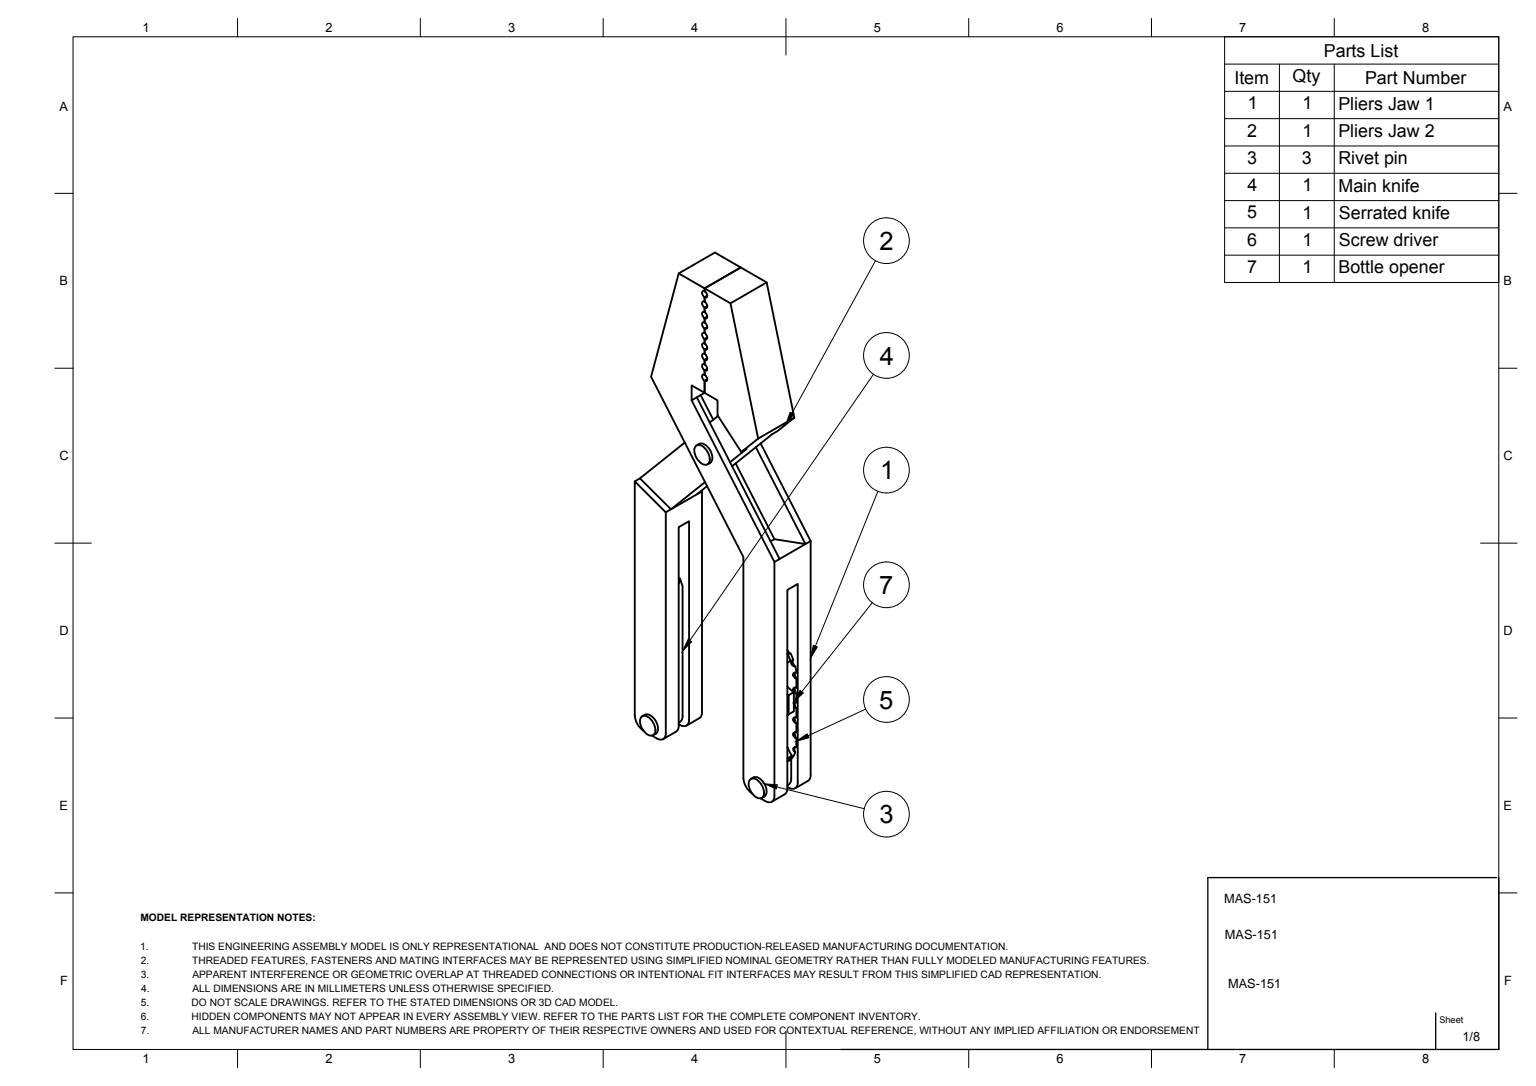
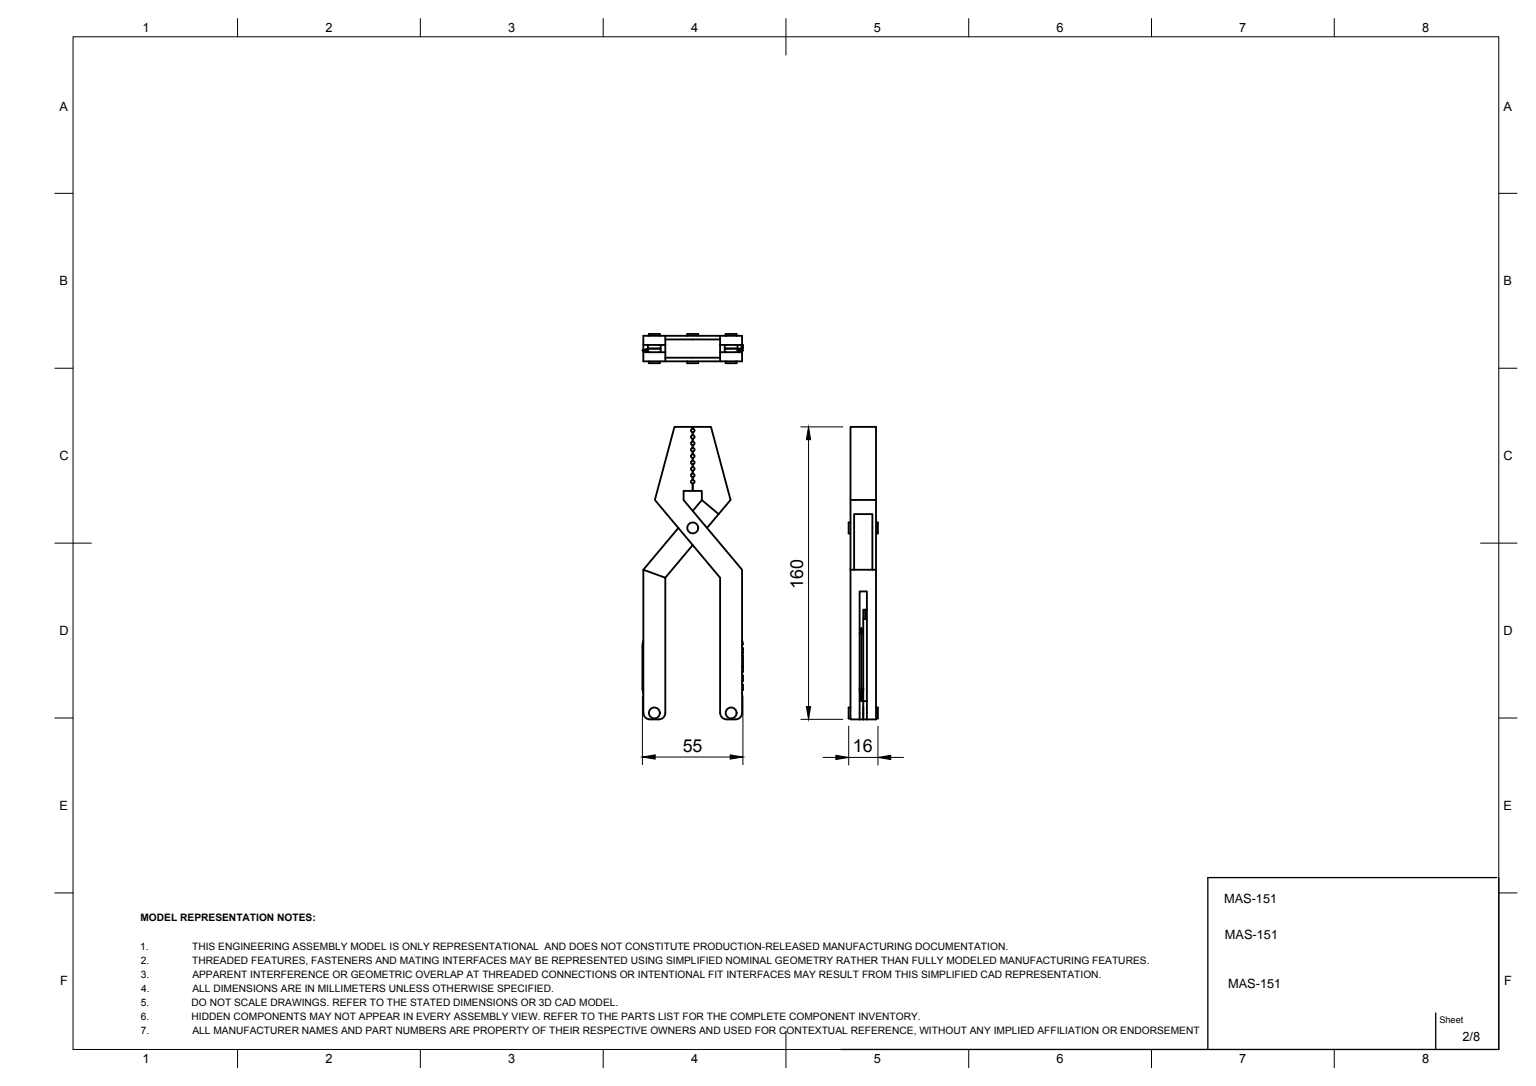
ISO-10303-21;
HEADER;
/* Generated by software containing ST-Developer
 * from STEP Tools, Inc. (www.steptools.com) 
 */

FILE_DESCRIPTION(
/* description */ ('STEP AP214'),
/* implementation_level */ '2;1');

FILE_NAME(
/* name */ 'MAS-151',
/* time_stamp */ '2026-11-04T19:14:12-08:00',
/* author */ (''),
/* organization */ (''),
/* preprocessor_version */ 'ST-DEVELOPER v20.2',
/* originating_system */ 'Autodesk Translation Framework v15.17.0.0',
/* authorisation */ '');

FILE_SCHEMA (('AUTOMOTIVE_DESIGN { 1 0 10303 214 3 1 1 }'));
ENDSEC;

DATA;
#10=MECHANICAL_DESIGN_GEOMETRIC_PRESENTATION_REPRESENTATION('',(#99,#100,
#101,#102,#103,#104,#105),#5990);
#11=ITEM_DEFINED_TRANSFORMATION($,$,#3355,#3676);
#12=ITEM_DEFINED_TRANSFORMATION($,$,#3437,#3677);
#13=ITEM_DEFINED_TRANSFORMATION($,$,#3662,#3678);
#14=ITEM_DEFINED_TRANSFORMATION($,$,#3519,#3679);
#15=ITEM_DEFINED_TRANSFORMATION($,$,#3540,#3680);
#16=ITEM_DEFINED_TRANSFORMATION($,$,#3585,#3681);
#17=ITEM_DEFINED_TRANSFORMATION($,$,#3638,#3682);
#18=ITEM_DEFINED_TRANSFORMATION($,$,#3662,#3683);
#19=ITEM_DEFINED_TRANSFORMATION($,$,#3662,#3684);
#20=(
REPRESENTATION_RELATIONSHIP($,$,#6021,#6020)
REPRESENTATION_RELATIONSHIP_WITH_TRANSFORMATION(#11)
SHAPE_REPRESENTATION_RELATIONSHIP()
);
#21=(
REPRESENTATION_RELATIONSHIP($,$,#6022,#6020)
REPRESENTATION_RELATIONSHIP_WITH_TRANSFORMATION(#12)
SHAPE_REPRESENTATION_RELATIONSHIP()
);
#22=(
REPRESENTATION_RELATIONSHIP($,$,#6027,#6020)
REPRESENTATION_RELATIONSHIP_WITH_TRANSFORMATION(#13)
SHAPE_REPRESENTATION_RELATIONSHIP()
);
#23=(
REPRESENTATION_RELATIONSHIP($,$,#6023,#6020)
REPRESENTATION_RELATIONSHIP_WITH_TRANSFORMATION(#14)
SHAPE_REPRESENTATION_RELATIONSHIP()
);
#24=(
REPRESENTATION_RELATIONSHIP($,$,#6024,#6020)
REPRESENTATION_RELATIONSHIP_WITH_TRANSFORMATION(#15)
SHAPE_REPRESENTATION_RELATIONSHIP()
);
#25=(
REPRESENTATION_RELATIONSHIP($,$,#6025,#6020)
REPRESENTATION_RELATIONSHIP_WITH_TRANSFORMATION(#16)
SHAPE_REPRESENTATION_RELATIONSHIP()
);
#26=(
REPRESENTATION_RELATIONSHIP($,$,#6026,#6020)
REPRESENTATION_RELATIONSHIP_WITH_TRANSFORMATION(#17)
SHAPE_REPRESENTATION_RELATIONSHIP()
);
#27=(
REPRESENTATION_RELATIONSHIP($,$,#6027,#6020)
REPRESENTATION_RELATIONSHIP_WITH_TRANSFORMATION(#18)
SHAPE_REPRESENTATION_RELATIONSHIP()
);
#28=(
REPRESENTATION_RELATIONSHIP($,$,#6027,#6020)
REPRESENTATION_RELATIONSHIP_WITH_TRANSFORMATION(#19)
SHAPE_REPRESENTATION_RELATIONSHIP()
);
#29=CONTEXT_DEPENDENT_SHAPE_REPRESENTATION(#20,#6011);
#30=CONTEXT_DEPENDENT_SHAPE_REPRESENTATION(#21,#6012);
#31=CONTEXT_DEPENDENT_SHAPE_REPRESENTATION(#22,#6013);
#32=CONTEXT_DEPENDENT_SHAPE_REPRESENTATION(#23,#6014);
#33=CONTEXT_DEPENDENT_SHAPE_REPRESENTATION(#24,#6015);
#34=CONTEXT_DEPENDENT_SHAPE_REPRESENTATION(#25,#6016);
#35=CONTEXT_DEPENDENT_SHAPE_REPRESENTATION(#26,#6017);
#36=CONTEXT_DEPENDENT_SHAPE_REPRESENTATION(#27,#6018);
#37=CONTEXT_DEPENDENT_SHAPE_REPRESENTATION(#28,#6019);
#38=NEXT_ASSEMBLY_USAGE_OCCURRENCE('Pliers Jaw 1:1','Pliers Jaw 1:1',
'Pliers Jaw 1:1',#6029,#6030,'Pliers Jaw 1:1');
#39=NEXT_ASSEMBLY_USAGE_OCCURRENCE('Pliers Jaw 2:1','Pliers Jaw 2:1',
'Pliers Jaw 2:1',#6029,#6031,'Pliers Jaw 2:1');
#40=NEXT_ASSEMBLY_USAGE_OCCURRENCE('rivet pin:1','rivet pin:1',
'rivet pin:1',#6029,#6036,'rivet pin:1');
#41=NEXT_ASSEMBLY_USAGE_OCCURRENCE('main knife:1','main knife:1',
'main knife:1',#6029,#6032,'main knife:1');
#42=NEXT_ASSEMBLY_USAGE_OCCURRENCE('serrated knife:1',
'serrated knife:1','serrated knife:1',#6029,#6033,'serrated knife:1');
#43=NEXT_ASSEMBLY_USAGE_OCCURRENCE('screw driver:1','screw driver:1',
'screw driver:1',#6029,#6034,'screw driver:1');
#44=NEXT_ASSEMBLY_USAGE_OCCURRENCE('bottle opener:1','bottle opener:1',
'bottle opener:1',#6029,#6035,'bottle opener:1');
#45=NEXT_ASSEMBLY_USAGE_OCCURRENCE('rivet pin:2','rivet pin:2',
'rivet pin:2',#6029,#6036,'rivet pin:2');
#46=NEXT_ASSEMBLY_USAGE_OCCURRENCE('rivet pin:3','rivet pin:3',
'rivet pin:3',#6029,#6036,'rivet pin:3');
#47=(
BOUNDED_SURFACE()
B_SPLINE_SURFACE(3,2,((#5769,#5770,#5771),(#5772,#5773,#5774),(#5775,#5776,
#5777),(#5778,#5779,#5780),(#5781,#5782,#5783),(#5784,#5785,#5786),(#5787,
#5788,#5789),(#5790,#5791,#5792),(#5793,#5794,#5795),(#5796,#5797,#5798),
(#5799,#5800,#5801),(#5802,#5803,#5804),(#5805,#5806,#5807),(#5808,#5809,
#5810),(#5811,#5812,#5813),(#5814,#5815,#5816),(#5817,#5818,#5819),(#5820,
#5821,#5822)),.UNSPECIFIED.,.F.,.F.,.F.)
B_SPLINE_SURFACE_WITH_KNOTS((4,2,2,2,2,2,2,2,4),(3,3),(0.00467154358091484,
0.00499795425216117,0.00521234917938639,0.00542674410661162,0.00564113903383685,
0.00585553396106207,0.0060699288882873,0.00628432381551252,0.00661073448675885),
(0.,1.00011201574402),.UNSPECIFIED.)
GEOMETRIC_REPRESENTATION_ITEM()
RATIONAL_B_SPLINE_SURFACE(((1.,0.701778016251575,1.00006681111479),(1.,
0.706507936356085,1.00006575146375),(1.,0.712393708374132,1.00006443286548),
(1.,0.724799452378116,1.00006165358819),(1.,0.730457055067376,1.00006038610704),
(1.,0.742658843750505,1.00005765252217),(1.,0.749286323952398,1.00005616775792),
(1.,0.759971140951244,1.00005377402247),(1.,0.763704964258696,1.00005293752847),
(1.,0.763766920917064,1.00005292364823),(1.,0.760086272902725,1.00005374822928),
(1.,0.74942657380375,1.00005613633753),(1.,0.742780641856394,1.00005762523556),
(1.,0.730540791311145,1.00006036734749),(1.,0.724865847327457,1.00006163871363),
(1.,0.712422254236158,1.00006442647031),(1.,0.706506681063795,1.00006575174497),
(1.,0.701749277073212,1.00006681755327)))
REPRESENTATION_ITEM('')
SURFACE()
);
#48=(
BOUNDED_SURFACE()
B_SPLINE_SURFACE(3,2,((#5827,#5828,#5829),(#5830,#5831,#5832),(#5833,#5834,
#5835),(#5836,#5837,#5838),(#5839,#5840,#5841),(#5842,#5843,#5844),(#5845,
#5846,#5847),(#5848,#5849,#5850),(#5851,#5852,#5853),(#5854,#5855,#5856),
(#5857,#5858,#5859),(#5860,#5861,#5862),(#5863,#5864,#5865),(#5866,#5867,
#5868),(#5869,#5870,#5871),(#5872,#5873,#5874),(#5875,#5876,#5877),(#5878,
#5879,#5880)),.UNSPECIFIED.,.F.,.F.,.F.)
B_SPLINE_SURFACE_WITH_KNOTS((4,2,2,2,2,2,2,2,4),(3,3),(0.00467154358091712,
0.00499795425216117,0.0052123491793864,0.00542674410661162,0.00564113903383685,
0.00585553396106207,0.0060699288882873,0.00628432381551253,0.00661073448675658),
(0.,1.00011201574402),.UNSPECIFIED.)
GEOMETRIC_REPRESENTATION_ITEM()
RATIONAL_B_SPLINE_SURFACE(((1.,0.701778016251691,1.00006681111478),(1.,
0.706507936356154,1.00006575146375),(1.,0.712393708374192,1.00006443286548),
(1.,0.724799452378113,1.00006165358819),(1.,0.730457055067361,1.00006038610704),
(1.,0.742658843750522,1.00005765252217),(1.,0.749286323952399,1.00005616775792),
(1.,0.759971140951245,1.00005377402246),(1.,0.763704964258696,1.00005293752847),
(1.,0.763766920917065,1.00005292364823),(1.,0.760086272902701,1.00005374822928),
(1.,0.749426573803775,1.00005613633753),(1.,0.742780641856403,1.00005762523556),
(1.,0.730540791311137,1.00006036734749),(1.,0.724865847327466,1.00006163871363),
(1.,0.712422254236199,1.00006442647031),(1.,0.706506681063906,1.00006575174497),
(1.,0.70174927707328,1.00006681755327)))
REPRESENTATION_ITEM('')
SURFACE()
);
#49=ELLIPSE('',#3546,1.05409255338808,0.99999999999868);
#50=ELLIPSE('',#3547,1.05409255338732,0.999999999998124);
#51=ELLIPSE('',#3549,1.05409255339022,1.00000000000065);
#52=ELLIPSE('',#3550,1.05409255338729,0.999999999997981);
#53=ELLIPSE('',#3552,1.05409255338844,0.99999999999902);
#54=ELLIPSE('',#3553,1.05409255338858,0.999999999999168);
#55=ELLIPSE('',#3555,1.05409255338794,0.999999999998691);
#56=ELLIPSE('',#3556,1.05409255338792,0.999999999998643);
#57=ELLIPSE('',#3558,1.05409255338783,0.999999999998475);
#58=ELLIPSE('',#3559,1.05409255338765,0.999999999998245);
#59=B_SPLINE_CURVE_WITH_KNOTS('',3,(#5264,#5265,#5266,#5267,#5268,#5269,
#5270,#5271,#5272,#5273,#5274,#5275,#5276,#5277,#5278,#5279,#5280,#5281),
 .UNSPECIFIED.,.F.,.F.,(4,2,2,2,2,2,2,2,4),(-0.601003528896593,-0.581975187755184,
-0.544665520692116,-0.509562261507989,-0.474459002323862,-0.439355743139737,
-0.404252483955611,-0.366942816892543,-0.347914475751133),.UNSPECIFIED.);
#60=B_SPLINE_CURVE_WITH_KNOTS('',3,(#5282,#5283,#5284,#5285,#5286,#5287,
#5288,#5289,#5290,#5291,#5292,#5293,#5294,#5295,#5296,#5297,#5298,#5299),
 .UNSPECIFIED.,.F.,.F.,(4,2,2,2,2,2,2,2,4),(-0.27137037906712,-0.252342037925712,
-0.215032370862644,-0.179929111678516,-0.144825852494388,-0.109722593310262,
-0.0746193341261349,-0.0373096670630674,-0.0182813259216579),
 .UNSPECIFIED.);
#61=B_SPLINE_CURVE_WITH_KNOTS('',3,(#5323,#5324,#5325,#5326,#5327,#5328,
#5329,#5330,#5331,#5332,#5333,#5334,#5335),.UNSPECIFIED.,.F.,.F.,(4,3,2,
2,2,4),(-0.00524378789543694,-6.24500451351651E-17,0.037252819941784,0.0745056398835681,
0.109553010570145,0.144600381256721),.UNSPECIFIED.);
#62=B_SPLINE_CURVE_WITH_KNOTS('',3,(#5340,#5341,#5342,#5343,#5344,#5345,
#5346,#5347,#5348,#5349,#5350,#5351,#5352),.UNSPECIFIED.,.F.,.F.,(4,2,2,
2,3,4),(-0.144600381256721,-0.109553010570144,-0.0745056398835681,-0.037252819941784,
5.55111512312578E-17,0.00524378789543793),.UNSPECIFIED.);
#63=B_SPLINE_CURVE_WITH_KNOTS('',3,(#5356,#5357,#5358,#5359,#5360,#5361,
#5362,#5363,#5364,#5365,#5366,#5367,#5368,#5369,#5370,#5371,#5372,#5373,
#5374,#5375,#5376,#5377,#5378),.UNSPECIFIED.,.F.,.F.,(4,3,2,2,2,2,2,2,2,
2,4),(-0.00524378789548939,0.,0.0372528199418273,0.0745056398836546,0.109553010570272,
0.144600381256889,0.179647751943506,0.214695122630123,0.25194794257195,
0.289200762513778,0.294444550409127),.UNSPECIFIED.);
#64=B_SPLINE_CURVE_WITH_KNOTS('',3,(#5379,#5380,#5381,#5382,#5383,#5384,
#5385,#5386,#5387,#5388,#5389,#5390,#5391,#5392,#5393,#5394,#5395,#5396,
#5397,#5398,#5399,#5400,#5401),.UNSPECIFIED.,.F.,.F.,(4,2,2,2,2,2,2,2,2,
3,4),(-0.294444550409266,-0.289200762513777,-0.25194794257195,-0.214695122630123,
-0.179647751943506,-0.144600381256889,-0.109553010570272,-0.0745056398836545,
-0.0372528199418273,0.,0.00524378789535096),.UNSPECIFIED.);
#65=B_SPLINE_CURVE_WITH_KNOTS('',3,(#5405,#5406,#5407,#5408,#5409,#5410,
#5411,#5412,#5413,#5414,#5415,#5416,#5417,#5418,#5419,#5420,#5421,#5422,
#5423,#5424,#5425,#5426,#5427),.UNSPECIFIED.,.F.,.F.,(4,3,2,2,2,2,2,2,2,
2,4),(-0.00524378789552401,0.,0.0372528199418277,0.0745056398836554,0.109553010570272,
0.144600381256889,0.179647751943506,0.214695122630123,0.25194794257195,
0.289200762513778,0.294444550409163),.UNSPECIFIED.);
#66=B_SPLINE_CURVE_WITH_KNOTS('',3,(#5428,#5429,#5430,#5431,#5432,#5433,
#5434,#5435,#5436,#5437,#5438,#5439,#5440,#5441,#5442,#5443,#5444,#5445,
#5446,#5447,#5448,#5449,#5450),.UNSPECIFIED.,.F.,.F.,(4,2,2,2,2,2,2,2,2,
3,4),(-0.294444550409303,-0.289200762513778,-0.25194794257195,-0.214695122630123,
-0.179647751943506,-0.144600381256889,-0.109553010570272,-0.0745056398836553,
-0.0372528199418277,0.,0.0052437878953856),.UNSPECIFIED.);
#67=B_SPLINE_CURVE_WITH_KNOTS('',3,(#5454,#5455,#5456,#5457,#5458,#5459,
#5460,#5461,#5462,#5463,#5464,#5465,#5466,#5467,#5468,#5469,#5470,#5471,
#5472,#5473,#5474,#5475,#5476),.UNSPECIFIED.,.F.,.F.,(4,3,2,2,2,2,2,2,2,
2,4),(-0.00524378789543961,0.,0.0372528199417981,0.0745056398835963,0.109553010570186,
0.144600381256775,0.179647751943365,0.214695122629955,0.251947942571753,
0.289200762513551,0.294444550408852),.UNSPECIFIED.);
#68=B_SPLINE_CURVE_WITH_KNOTS('',3,(#5477,#5478,#5479,#5480,#5481,#5482,
#5483,#5484,#5485,#5486,#5487,#5488,#5489,#5490,#5491,#5492,#5493,#5494,
#5495,#5496,#5497,#5498,#5499),.UNSPECIFIED.,.F.,.F.,(4,2,2,2,2,2,2,2,2,
3,4),(-0.294444550408994,-0.289200762513552,-0.251947942571754,-0.214695122629956,
-0.179647751943366,-0.144600381256776,-0.109553010570186,-0.0745056398835967,
-0.0372528199417983,0.,0.00524378789530167),.UNSPECIFIED.);
#69=B_SPLINE_CURVE_WITH_KNOTS('',3,(#5554,#5555,#5556,#5557,#5558,#5559,
#5560,#5561,#5562,#5563,#5564,#5565),.UNSPECIFIED.,.F.,.F.,(4,2,2,2,2,4),
(-0.294444550409229,-0.289200762513778,-0.251947942571951,-0.214695122630124,
-0.179647751943506,-0.144600381256889),.UNSPECIFIED.);
#70=B_SPLINE_CURVE_WITH_KNOTS('',3,(#5573,#5574,#5575,#5576,#5577,#5578,
#5579,#5580,#5581,#5582,#5583,#5584),.UNSPECIFIED.,.F.,.F.,(4,2,2,2,2,4),
(-0.474692173414376,-0.439644802727758,-0.404597432041141,-0.367344612099314,
-0.330091792157487,-0.324848004262036),.UNSPECIFIED.);
#71=B_SPLINE_CURVE_WITH_KNOTS('',3,(#5643,#5644,#5645,#5646,#5647,#5648,
#5649,#5650,#5651,#5652,#5653,#5654,#5655,#5656,#5657,#5658,#5659,#5660,
#5661,#5662,#5663,#5664,#5665,#5666,#5667),.UNSPECIFIED.,.F.,.F.,(4,3,3,
3,3,3,3,3,4),(0.,0.000216694552239529,0.00043295736495498,0.000650463962575776,
0.00086591472990996,0.00108361531562917,0.00129887209486494,0.00151612908143691,
0.00173182945981992),.UNSPECIFIED.);
#72=B_SPLINE_CURVE_WITH_KNOTS('',3,(#5680,#5681,#5682,#5683,#5684,#5685,
#5686,#5687,#5688,#5689,#5690,#5691,#5692,#5693,#5694,#5695,#5696,#5697,
#5698,#5699,#5700,#5701,#5702,#5703,#5704),.UNSPECIFIED.,.F.,.F.,(4,3,3,
3,3,3,3,3,4),(0.,0.000216694552239523,0.00043295736495498,0.000650463962575778,
0.00086591472990996,0.00108361531562917,0.00129887209486494,0.00151612908143692,
0.00173182945981992),.UNSPECIFIED.);
#73=CONICAL_SURFACE('',#3531,6.99999999999997,1.24904577239826);
#74=CONICAL_SURFACE('',#3534,6.99999999999997,1.24904577239826);
#75=CONICAL_SURFACE('',#3535,6.99999999999997,1.24904577239826);
#76=CONICAL_SURFACE('',#3538,6.99999999999997,1.24904577239826);
#77=CONICAL_SURFACE('',#3571,6.99999999999997,1.24904577239826);
#78=CONICAL_SURFACE('',#3575,6.99999999999997,1.24904577239826);
#79=CONICAL_SURFACE('',#3576,6.99999999999997,1.24904577239826);
#80=CONICAL_SURFACE('',#3582,6.99999999999997,1.24904577239826);
#81=(
BOUNDED_CURVE()
B_SPLINE_CURVE(2,(#5211,#5212,#5213),.UNSPECIFIED.,.F.,.F.)
B_SPLINE_CURVE_WITH_KNOTS((3,3),(1.46969384566992,2.45666783066589),
 .UNSPECIFIED.)
CURVE()
GEOMETRIC_REPRESENTATION_ITEM()
RATIONAL_B_SPLINE_CURVE((1.64285714285714,1.64285714285714,1.35294117647059))
REPRESENTATION_ITEM('')
);
#82=(
BOUNDED_CURVE()
B_SPLINE_CURVE(2,(#5214,#5215,#5216),.UNSPECIFIED.,.F.,.F.)
B_SPLINE_CURVE_WITH_KNOTS((3,3),(0.482719860673933,1.46969384566992),
 .UNSPECIFIED.)
CURVE()
GEOMETRIC_REPRESENTATION_ITEM()
RATIONAL_B_SPLINE_CURVE((1.35294117647058,1.64285714285714,1.64285714285714))
REPRESENTATION_ITEM('')
);
#83=(
BOUNDED_CURVE()
B_SPLINE_CURVE(2,(#5509,#5510,#5511),.UNSPECIFIED.,.F.,.F.)
B_SPLINE_CURVE_WITH_KNOTS((3,3),(1.46969384566992,2.45666783066588),
 .UNSPECIFIED.)
CURVE()
GEOMETRIC_REPRESENTATION_ITEM()
RATIONAL_B_SPLINE_CURVE((1.64285714285715,1.64285714285715,1.35294117647059))
REPRESENTATION_ITEM('')
);
#84=(
BOUNDED_CURVE()
B_SPLINE_CURVE(2,(#5512,#5513,#5514),.UNSPECIFIED.,.F.,.F.)
B_SPLINE_CURVE_WITH_KNOTS((3,3),(0.482719860673934,1.46969384566991),
 .UNSPECIFIED.)
CURVE()
GEOMETRIC_REPRESENTATION_ITEM()
RATIONAL_B_SPLINE_CURVE((1.35294117647058,1.64285714285714,1.64285714285714))
REPRESENTATION_ITEM('')
);
#85=SHAPE_REPRESENTATION_RELATIONSHIP('SRR','None',#6021,#92);
#86=SHAPE_REPRESENTATION_RELATIONSHIP('SRR','None',#6022,#93);
#87=SHAPE_REPRESENTATION_RELATIONSHIP('SRR','None',#6023,#94);
#88=SHAPE_REPRESENTATION_RELATIONSHIP('SRR','None',#6024,#95);
#89=SHAPE_REPRESENTATION_RELATIONSHIP('SRR','None',#6025,#96);
#90=SHAPE_REPRESENTATION_RELATIONSHIP('SRR','None',#6026,#97);
#91=SHAPE_REPRESENTATION_RELATIONSHIP('SRR','None',#6027,#98);
#92=ADVANCED_BREP_SHAPE_REPRESENTATION('',(#106),#5983);
#93=ADVANCED_BREP_SHAPE_REPRESENTATION('',(#107),#5984);
#94=ADVANCED_BREP_SHAPE_REPRESENTATION('',(#108),#5985);
#95=ADVANCED_BREP_SHAPE_REPRESENTATION('',(#109),#5986);
#96=ADVANCED_BREP_SHAPE_REPRESENTATION('',(#110),#5987);
#97=ADVANCED_BREP_SHAPE_REPRESENTATION('',(#111),#5988);
#98=ADVANCED_BREP_SHAPE_REPRESENTATION('',(#112),#5989);
#99=STYLED_ITEM('',(#6065),#106);
#100=STYLED_ITEM('',(#6065),#107);
#101=STYLED_ITEM('',(#6066),#108);
#102=STYLED_ITEM('',(#6066),#109);
#103=STYLED_ITEM('',(#6067),#110);
#104=STYLED_ITEM('',(#6068),#111);
#105=STYLED_ITEM('',(#6069),#112);
#106=MANIFOLD_SOLID_BREP('Body1',#3269);
#107=MANIFOLD_SOLID_BREP('Body1',#3270);
#108=MANIFOLD_SOLID_BREP('Body1',#3271);
#109=MANIFOLD_SOLID_BREP('Body1',#3272);
#110=MANIFOLD_SOLID_BREP('Body1',#3273);
#111=MANIFOLD_SOLID_BREP('Body1',#3274);
#112=MANIFOLD_SOLID_BREP('Body1',#3275);
#113=FACE_BOUND('',#427,.T.);
#114=FACE_BOUND('',#428,.T.);
#115=FACE_BOUND('',#430,.T.);
#116=FACE_BOUND('',#431,.T.);
#117=FACE_BOUND('',#463,.T.);
#118=FACE_BOUND('',#465,.T.);
#119=FACE_BOUND('',#467,.T.);
#120=FACE_BOUND('',#469,.T.);
#121=FACE_BOUND('',#479,.T.);
#122=FACE_BOUND('',#484,.T.);
#123=FACE_BOUND('',#516,.T.);
#124=FACE_BOUND('',#520,.T.);
#125=FACE_BOUND('',#522,.T.);
#126=FACE_BOUND('',#524,.T.);
#127=FACE_BOUND('',#534,.T.);
#128=FACE_BOUND('',#536,.T.);
#129=FACE_BOUND('',#557,.T.);
#130=FACE_BOUND('',#559,.T.);
#131=FACE_BOUND('',#577,.T.);
#132=FACE_BOUND('',#579,.T.);
#133=FACE_BOUND('',#604,.T.);
#134=FACE_BOUND('',#606,.T.);
#135=FACE_BOUND('',#618,.T.);
#136=FACE_BOUND('',#621,.T.);
#137=PLANE('',#3368);
#138=PLANE('',#3369);
#139=PLANE('',#3370);
#140=PLANE('',#3382);
#141=PLANE('',#3394);
#142=PLANE('',#3395);
#143=PLANE('',#3396);
#144=PLANE('',#3397);
#145=PLANE('',#3398);
#146=PLANE('',#3399);
#147=PLANE('',#3400);
#148=PLANE('',#3401);
#149=PLANE('',#3402);
#150=PLANE('',#3403);
#151=PLANE('',#3404);
#152=PLANE('',#3405);
#153=PLANE('',#3406);
#154=PLANE('',#3407);
#155=PLANE('',#3408);
#156=PLANE('',#3409);
#157=PLANE('',#3410);
#158=PLANE('',#3411);
#159=PLANE('',#3412);
#160=PLANE('',#3422);
#161=PLANE('',#3423);
#162=PLANE('',#3424);
#163=PLANE('',#3425);
#164=PLANE('',#3426);
#165=PLANE('',#3429);
#166=PLANE('',#3432);
#167=PLANE('',#3447);
#168=PLANE('',#3450);
#169=PLANE('',#3451);
#170=PLANE('',#3452);
#171=PLANE('',#3462);
#172=PLANE('',#3465);
#173=PLANE('',#3466);
#174=PLANE('',#3476);
#175=PLANE('',#3477);
#176=PLANE('',#3478);
#177=PLANE('',#3479);
#178=PLANE('',#3480);
#179=PLANE('',#3481);
#180=PLANE('',#3482);
#181=PLANE('',#3483);
#182=PLANE('',#3484);
#183=PLANE('',#3485);
#184=PLANE('',#3486);
#185=PLANE('',#3487);
#186=PLANE('',#3488);
#187=PLANE('',#3489);
#188=PLANE('',#3490);
#189=PLANE('',#3491);
#190=PLANE('',#3492);
#191=PLANE('',#3502);
#192=PLANE('',#3503);
#193=PLANE('',#3504);
#194=PLANE('',#3505);
#195=PLANE('',#3506);
#196=PLANE('',#3507);
#197=PLANE('',#3508);
#198=PLANE('',#3511);
#199=PLANE('',#3514);
#200=PLANE('',#3523);
#201=PLANE('',#3524);
#202=PLANE('',#3525);
#203=PLANE('',#3528);
#204=PLANE('',#3533);
#205=PLANE('',#3537);
#206=PLANE('',#3563);
#207=PLANE('',#3564);
#208=PLANE('',#3565);
#209=PLANE('',#3568);
#210=PLANE('',#3574);
#211=PLANE('',#3581);
#212=PLANE('',#3602);
#213=PLANE('',#3603);
#214=PLANE('',#3604);
#215=PLANE('',#3605);
#216=PLANE('',#3606);
#217=PLANE('',#3607);
#218=PLANE('',#3608);
#219=PLANE('',#3612);
#220=PLANE('',#3616);
#221=PLANE('',#3617);
#222=PLANE('',#3618);
#223=PLANE('',#3619);
#224=PLANE('',#3620);
#225=PLANE('',#3621);
#226=PLANE('',#3622);
#227=PLANE('',#3623);
#228=PLANE('',#3624);
#229=PLANE('',#3625);
#230=PLANE('',#3626);
#231=PLANE('',#3627);
#232=PLANE('',#3628);
#233=PLANE('',#3648);
#234=PLANE('',#3652);
#235=PLANE('',#3656);
#236=PLANE('',#3657);
#237=PLANE('',#3658);
#238=PLANE('',#3672);
#239=PLANE('',#3673);
#240=PLANE('',#3674);
#241=PLANE('',#3675);
#242=FACE_OUTER_BOUND('',#420,.T.);
#243=FACE_OUTER_BOUND('',#421,.T.);
#244=FACE_OUTER_BOUND('',#422,.T.);
#245=FACE_OUTER_BOUND('',#423,.T.);
#246=FACE_OUTER_BOUND('',#424,.T.);
#247=FACE_OUTER_BOUND('',#425,.T.);
#248=FACE_OUTER_BOUND('',#426,.T.);
#249=FACE_OUTER_BOUND('',#429,.T.);
#250=FACE_OUTER_BOUND('',#432,.T.);
#251=FACE_OUTER_BOUND('',#433,.T.);
#252=FACE_OUTER_BOUND('',#434,.T.);
#253=FACE_OUTER_BOUND('',#435,.T.);
#254=FACE_OUTER_BOUND('',#436,.T.);
#255=FACE_OUTER_BOUND('',#437,.T.);
#256=FACE_OUTER_BOUND('',#438,.T.);
#257=FACE_OUTER_BOUND('',#439,.T.);
#258=FACE_OUTER_BOUND('',#440,.T.);
#259=FACE_OUTER_BOUND('',#441,.T.);
#260=FACE_OUTER_BOUND('',#442,.T.);
#261=FACE_OUTER_BOUND('',#443,.T.);
#262=FACE_OUTER_BOUND('',#444,.T.);
#263=FACE_OUTER_BOUND('',#445,.T.);
#264=FACE_OUTER_BOUND('',#446,.T.);
#265=FACE_OUTER_BOUND('',#447,.T.);
#266=FACE_OUTER_BOUND('',#448,.T.);
#267=FACE_OUTER_BOUND('',#449,.T.);
#268=FACE_OUTER_BOUND('',#450,.T.);
#269=FACE_OUTER_BOUND('',#451,.T.);
#270=FACE_OUTER_BOUND('',#452,.T.);
#271=FACE_OUTER_BOUND('',#453,.T.);
#272=FACE_OUTER_BOUND('',#454,.T.);
#273=FACE_OUTER_BOUND('',#455,.T.);
#274=FACE_OUTER_BOUND('',#456,.T.);
#275=FACE_OUTER_BOUND('',#457,.T.);
#276=FACE_OUTER_BOUND('',#458,.T.);
#277=FACE_OUTER_BOUND('',#459,.T.);
#278=FACE_OUTER_BOUND('',#460,.T.);
#279=FACE_OUTER_BOUND('',#461,.T.);
#280=FACE_OUTER_BOUND('',#462,.T.);
#281=FACE_OUTER_BOUND('',#464,.T.);
#282=FACE_OUTER_BOUND('',#466,.T.);
#283=FACE_OUTER_BOUND('',#468,.T.);
#284=FACE_OUTER_BOUND('',#470,.T.);
#285=FACE_OUTER_BOUND('',#471,.T.);
#286=FACE_OUTER_BOUND('',#472,.T.);
#287=FACE_OUTER_BOUND('',#473,.T.);
#288=FACE_OUTER_BOUND('',#474,.T.);
#289=FACE_OUTER_BOUND('',#475,.T.);
#290=FACE_OUTER_BOUND('',#476,.T.);
#291=FACE_OUTER_BOUND('',#477,.T.);
#292=FACE_OUTER_BOUND('',#478,.T.);
#293=FACE_OUTER_BOUND('',#480,.T.);
#294=FACE_OUTER_BOUND('',#481,.T.);
#295=FACE_OUTER_BOUND('',#482,.T.);
#296=FACE_OUTER_BOUND('',#483,.T.);
#297=FACE_OUTER_BOUND('',#485,.T.);
#298=FACE_OUTER_BOUND('',#486,.T.);
#299=FACE_OUTER_BOUND('',#487,.T.);
#300=FACE_OUTER_BOUND('',#488,.T.);
#301=FACE_OUTER_BOUND('',#489,.T.);
#302=FACE_OUTER_BOUND('',#490,.T.);
#303=FACE_OUTER_BOUND('',#491,.T.);
#304=FACE_OUTER_BOUND('',#492,.T.);
#305=FACE_OUTER_BOUND('',#493,.T.);
#306=FACE_OUTER_BOUND('',#494,.T.);
#307=FACE_OUTER_BOUND('',#495,.T.);
#308=FACE_OUTER_BOUND('',#496,.T.);
#309=FACE_OUTER_BOUND('',#497,.T.);
#310=FACE_OUTER_BOUND('',#498,.T.);
#311=FACE_OUTER_BOUND('',#499,.T.);
#312=FACE_OUTER_BOUND('',#500,.T.);
#313=FACE_OUTER_BOUND('',#501,.T.);
#314=FACE_OUTER_BOUND('',#502,.T.);
#315=FACE_OUTER_BOUND('',#503,.T.);
#316=FACE_OUTER_BOUND('',#504,.T.);
#317=FACE_OUTER_BOUND('',#505,.T.);
#318=FACE_OUTER_BOUND('',#506,.T.);
#319=FACE_OUTER_BOUND('',#507,.T.);
#320=FACE_OUTER_BOUND('',#508,.T.);
#321=FACE_OUTER_BOUND('',#509,.T.);
#322=FACE_OUTER_BOUND('',#510,.T.);
#323=FACE_OUTER_BOUND('',#511,.T.);
#324=FACE_OUTER_BOUND('',#512,.T.);
#325=FACE_OUTER_BOUND('',#513,.T.);
#326=FACE_OUTER_BOUND('',#514,.T.);
#327=FACE_OUTER_BOUND('',#515,.T.);
#328=FACE_OUTER_BOUND('',#517,.T.);
#329=FACE_OUTER_BOUND('',#518,.T.);
#330=FACE_OUTER_BOUND('',#519,.T.);
#331=FACE_OUTER_BOUND('',#521,.T.);
#332=FACE_OUTER_BOUND('',#523,.T.);
#333=FACE_OUTER_BOUND('',#525,.T.);
#334=FACE_OUTER_BOUND('',#526,.T.);
#335=FACE_OUTER_BOUND('',#527,.T.);
#336=FACE_OUTER_BOUND('',#528,.T.);
#337=FACE_OUTER_BOUND('',#529,.T.);
#338=FACE_OUTER_BOUND('',#530,.T.);
#339=FACE_OUTER_BOUND('',#531,.T.);
#340=FACE_OUTER_BOUND('',#532,.T.);
#341=FACE_OUTER_BOUND('',#533,.T.);
#342=FACE_OUTER_BOUND('',#535,.T.);
#343=FACE_OUTER_BOUND('',#537,.T.);
#344=FACE_OUTER_BOUND('',#538,.T.);
#345=FACE_OUTER_BOUND('',#539,.T.);
#346=FACE_OUTER_BOUND('',#540,.T.);
#347=FACE_OUTER_BOUND('',#541,.T.);
#348=FACE_OUTER_BOUND('',#542,.T.);
#349=FACE_OUTER_BOUND('',#543,.T.);
#350=FACE_OUTER_BOUND('',#544,.T.);
#351=FACE_OUTER_BOUND('',#545,.T.);
#352=FACE_OUTER_BOUND('',#546,.T.);
#353=FACE_OUTER_BOUND('',#547,.T.);
#354=FACE_OUTER_BOUND('',#548,.T.);
#355=FACE_OUTER_BOUND('',#549,.T.);
#356=FACE_OUTER_BOUND('',#550,.T.);
#357=FACE_OUTER_BOUND('',#551,.T.);
#358=FACE_OUTER_BOUND('',#552,.T.);
#359=FACE_OUTER_BOUND('',#553,.T.);
#360=FACE_OUTER_BOUND('',#554,.T.);
#361=FACE_OUTER_BOUND('',#555,.T.);
#362=FACE_OUTER_BOUND('',#556,.T.);
#363=FACE_OUTER_BOUND('',#558,.T.);
#364=FACE_OUTER_BOUND('',#560,.T.);
#365=FACE_OUTER_BOUND('',#561,.T.);
#366=FACE_OUTER_BOUND('',#562,.T.);
#367=FACE_OUTER_BOUND('',#563,.T.);
#368=FACE_OUTER_BOUND('',#564,.T.);
#369=FACE_OUTER_BOUND('',#565,.T.);
#370=FACE_OUTER_BOUND('',#566,.T.);
#371=FACE_OUTER_BOUND('',#567,.T.);
#372=FACE_OUTER_BOUND('',#568,.T.);
#373=FACE_OUTER_BOUND('',#569,.T.);
#374=FACE_OUTER_BOUND('',#570,.T.);
#375=FACE_OUTER_BOUND('',#571,.T.);
#376=FACE_OUTER_BOUND('',#572,.T.);
#377=FACE_OUTER_BOUND('',#573,.T.);
#378=FACE_OUTER_BOUND('',#574,.T.);
#379=FACE_OUTER_BOUND('',#575,.T.);
#380=FACE_OUTER_BOUND('',#576,.T.);
#381=FACE_OUTER_BOUND('',#578,.T.);
#382=FACE_OUTER_BOUND('',#580,.T.);
#383=FACE_OUTER_BOUND('',#581,.T.);
#384=FACE_OUTER_BOUND('',#582,.T.);
#385=FACE_OUTER_BOUND('',#583,.T.);
#386=FACE_OUTER_BOUND('',#584,.T.);
#387=FACE_OUTER_BOUND('',#585,.T.);
#388=FACE_OUTER_BOUND('',#586,.T.);
#389=FACE_OUTER_BOUND('',#587,.T.);
#390=FACE_OUTER_BOUND('',#588,.T.);
#391=FACE_OUTER_BOUND('',#589,.T.);
#392=FACE_OUTER_BOUND('',#590,.T.);
#393=FACE_OUTER_BOUND('',#591,.T.);
#394=FACE_OUTER_BOUND('',#592,.T.);
#395=FACE_OUTER_BOUND('',#593,.T.);
#396=FACE_OUTER_BOUND('',#594,.T.);
#397=FACE_OUTER_BOUND('',#595,.T.);
#398=FACE_OUTER_BOUND('',#596,.T.);
#399=FACE_OUTER_BOUND('',#597,.T.);
#400=FACE_OUTER_BOUND('',#598,.T.);
#401=FACE_OUTER_BOUND('',#599,.T.);
#402=FACE_OUTER_BOUND('',#600,.T.);
#403=FACE_OUTER_BOUND('',#601,.T.);
#404=FACE_OUTER_BOUND('',#602,.T.);
#405=FACE_OUTER_BOUND('',#603,.T.);
#406=FACE_OUTER_BOUND('',#605,.T.);
#407=FACE_OUTER_BOUND('',#607,.T.);
#408=FACE_OUTER_BOUND('',#608,.T.);
#409=FACE_OUTER_BOUND('',#609,.T.);
#410=FACE_OUTER_BOUND('',#610,.T.);
#411=FACE_OUTER_BOUND('',#611,.T.);
#412=FACE_OUTER_BOUND('',#612,.T.);
#413=FACE_OUTER_BOUND('',#613,.T.);
#414=FACE_OUTER_BOUND('',#614,.T.);
#415=FACE_OUTER_BOUND('',#615,.T.);
#416=FACE_OUTER_BOUND('',#616,.T.);
#417=FACE_OUTER_BOUND('',#617,.T.);
#418=FACE_OUTER_BOUND('',#619,.T.);
#419=FACE_OUTER_BOUND('',#620,.T.);
#420=EDGE_LOOP('',(#2110,#2111,#2112,#2113));
#421=EDGE_LOOP('',(#2114,#2115,#2116,#2117));
#422=EDGE_LOOP('',(#2118,#2119,#2120,#2121));
#423=EDGE_LOOP('',(#2122,#2123,#2124,#2125));
#424=EDGE_LOOP('',(#2126,#2127,#2128,#2129));
#425=EDGE_LOOP('',(#2130,#2131,#2132,#2133));
#426=EDGE_LOOP('',(#2134,#2135,#2136,#2137,#2138,#2139,#2140,#2141,#2142,
#2143,#2144,#2145,#2146,#2147,#2148,#2149,#2150,#2151,#2152,#2153,#2154,
#2155,#2156,#2157,#2158,#2159,#2160,#2161,#2162,#2163));
#427=EDGE_LOOP('',(#2164));
#428=EDGE_LOOP('',(#2165));
#429=EDGE_LOOP('',(#2166,#2167,#2168,#2169,#2170,#2171,#2172,#2173,#2174,
#2175,#2176,#2177,#2178,#2179,#2180,#2181,#2182,#2183,#2184,#2185,#2186,
#2187,#2188,#2189,#2190,#2191,#2192,#2193,#2194,#2195));
#430=EDGE_LOOP('',(#2196));
#431=EDGE_LOOP('',(#2197));
#432=EDGE_LOOP('',(#2198,#2199,#2200,#2201));
#433=EDGE_LOOP('',(#2202,#2203,#2204,#2205));
#434=EDGE_LOOP('',(#2206,#2207,#2208,#2209));
#435=EDGE_LOOP('',(#2210,#2211,#2212,#2213));
#436=EDGE_LOOP('',(#2214,#2215,#2216,#2217));
#437=EDGE_LOOP('',(#2218,#2219,#2220,#2221));
#438=EDGE_LOOP('',(#2222,#2223,#2224,#2225));
#439=EDGE_LOOP('',(#2226,#2227,#2228,#2229));
#440=EDGE_LOOP('',(#2230,#2231,#2232,#2233));
#441=EDGE_LOOP('',(#2234,#2235,#2236,#2237,#2238,#2239));
#442=EDGE_LOOP('',(#2240,#2241,#2242,#2243));
#443=EDGE_LOOP('',(#2244,#2245,#2246,#2247));
#444=EDGE_LOOP('',(#2248,#2249,#2250,#2251));
#445=EDGE_LOOP('',(#2252,#2253,#2254,#2255,#2256,#2257,#2258,#2259));
#446=EDGE_LOOP('',(#2260,#2261,#2262,#2263,#2264,#2265,#2266,#2267,#2268,
#2269));
#447=EDGE_LOOP('',(#2270,#2271,#2272,#2273));
#448=EDGE_LOOP('',(#2274,#2275,#2276,#2277,#2278,#2279,#2280,#2281,#2282,
#2283));
#449=EDGE_LOOP('',(#2284,#2285,#2286,#2287));
#450=EDGE_LOOP('',(#2288,#2289,#2290,#2291));
#451=EDGE_LOOP('',(#2292,#2293,#2294,#2295));
#452=EDGE_LOOP('',(#2296,#2297,#2298,#2299));
#453=EDGE_LOOP('',(#2300,#2301,#2302,#2303));
#454=EDGE_LOOP('',(#2304,#2305,#2306,#2307));
#455=EDGE_LOOP('',(#2308,#2309,#2310,#2311));
#456=EDGE_LOOP('',(#2312,#2313,#2314,#2315));
#457=EDGE_LOOP('',(#2316,#2317,#2318,#2319));
#458=EDGE_LOOP('',(#2320,#2321,#2322,#2323));
#459=EDGE_LOOP('',(#2324,#2325,#2326,#2327));
#460=EDGE_LOOP('',(#2328,#2329,#2330,#2331));
#461=EDGE_LOOP('',(#2332,#2333,#2334,#2335));
#462=EDGE_LOOP('',(#2336,#2337,#2338,#2339));
#463=EDGE_LOOP('',(#2340));
#464=EDGE_LOOP('',(#2341,#2342,#2343,#2344));
#465=EDGE_LOOP('',(#2345));
#466=EDGE_LOOP('',(#2346,#2347,#2348,#2349,#2350,#2351));
#467=EDGE_LOOP('',(#2352));
#468=EDGE_LOOP('',(#2353,#2354,#2355,#2356,#2357,#2358));
#469=EDGE_LOOP('',(#2359));
#470=EDGE_LOOP('',(#2360,#2361,#2362,#2363));
#471=EDGE_LOOP('',(#2364,#2365,#2366,#2367));
#472=EDGE_LOOP('',(#2368,#2369,#2370,#2371));
#473=EDGE_LOOP('',(#2372,#2373,#2374,#2375));
#474=EDGE_LOOP('',(#2376,#2377,#2378,#2379));
#475=EDGE_LOOP('',(#2380,#2381,#2382,#2383));
#476=EDGE_LOOP('',(#2384,#2385,#2386,#2387));
#477=EDGE_LOOP('',(#2388,#2389,#2390,#2391));
#478=EDGE_LOOP('',(#2392,#2393,#2394,#2395,#2396,#2397));
#479=EDGE_LOOP('',(#2398));
#480=EDGE_LOOP('',(#2399,#2400,#2401,#2402));
#481=EDGE_LOOP('',(#2403,#2404,#2405,#2406,#2407,#2408,#2409,#2410));
#482=EDGE_LOOP('',(#2411,#2412,#2413,#2414,#2415,#2416,#2417,#2418,#2419,
#2420,#2421,#2422,#2423,#2424,#2425,#2426,#2427,#2428,#2429,#2430,#2431,
#2432,#2433,#2434,#2435));
#483=EDGE_LOOP('',(#2436,#2437,#2438,#2439,#2440,#2441));
#484=EDGE_LOOP('',(#2442));
#485=EDGE_LOOP('',(#2443,#2444,#2445,#2446));
#486=EDGE_LOOP('',(#2447,#2448,#2449,#2450,#2451,#2452,#2453,#2454,#2455,
#2456,#2457,#2458,#2459,#2460,#2461,#2462,#2463,#2464,#2465,#2466,#2467,
#2468,#2469,#2470,#2471));
#487=EDGE_LOOP('',(#2472,#2473,#2474,#2475));
#488=EDGE_LOOP('',(#2476,#2477,#2478,#2479));
#489=EDGE_LOOP('',(#2480,#2481,#2482,#2483));
#490=EDGE_LOOP('',(#2484,#2485,#2486,#2487));
#491=EDGE_LOOP('',(#2488,#2489,#2490,#2491));
#492=EDGE_LOOP('',(#2492,#2493,#2494,#2495));
#493=EDGE_LOOP('',(#2496,#2497,#2498,#2499));
#494=EDGE_LOOP('',(#2500,#2501,#2502,#2503));
#495=EDGE_LOOP('',(#2504,#2505,#2506,#2507));
#496=EDGE_LOOP('',(#2508,#2509,#2510,#2511,#2512,#2513));
#497=EDGE_LOOP('',(#2514,#2515,#2516,#2517));
#498=EDGE_LOOP('',(#2518,#2519,#2520,#2521));
#499=EDGE_LOOP('',(#2522,#2523,#2524,#2525,#2526,#2527,#2528,#2529,#2530,
#2531));
#500=EDGE_LOOP('',(#2532,#2533,#2534,#2535));
#501=EDGE_LOOP('',(#2536,#2537,#2538,#2539,#2540,#2541,#2542,#2543,#2544,
#2545));
#502=EDGE_LOOP('',(#2546,#2547,#2548,#2549));
#503=EDGE_LOOP('',(#2550,#2551,#2552,#2553));
#504=EDGE_LOOP('',(#2554,#2555,#2556,#2557));
#505=EDGE_LOOP('',(#2558,#2559,#2560,#2561));
#506=EDGE_LOOP('',(#2562,#2563,#2564,#2565));
#507=EDGE_LOOP('',(#2566,#2567,#2568,#2569));
#508=EDGE_LOOP('',(#2570,#2571,#2572,#2573));
#509=EDGE_LOOP('',(#2574,#2575,#2576,#2577));
#510=EDGE_LOOP('',(#2578,#2579,#2580,#2581));
#511=EDGE_LOOP('',(#2582,#2583,#2584,#2585));
#512=EDGE_LOOP('',(#2586,#2587,#2588,#2589));
#513=EDGE_LOOP('',(#2590,#2591,#2592,#2593));
#514=EDGE_LOOP('',(#2594,#2595,#2596,#2597));
#515=EDGE_LOOP('',(#2598,#2599,#2600,#2601));
#516=EDGE_LOOP('',(#2602));
#517=EDGE_LOOP('',(#2603,#2604,#2605,#2606));
#518=EDGE_LOOP('',(#2607,#2608,#2609,#2610));
#519=EDGE_LOOP('',(#2611,#2612,#2613,#2614));
#520=EDGE_LOOP('',(#2615));
#521=EDGE_LOOP('',(#2616,#2617,#2618,#2619,#2620,#2621));
#522=EDGE_LOOP('',(#2622));
#523=EDGE_LOOP('',(#2623,#2624,#2625,#2626,#2627,#2628));
#524=EDGE_LOOP('',(#2629));
#525=EDGE_LOOP('',(#2630,#2631,#2632,#2633));
#526=EDGE_LOOP('',(#2634,#2635,#2636,#2637));
#527=EDGE_LOOP('',(#2638,#2639,#2640,#2641));
#528=EDGE_LOOP('',(#2642,#2643,#2644,#2645));
#529=EDGE_LOOP('',(#2646,#2647,#2648,#2649));
#530=EDGE_LOOP('',(#2650,#2651,#2652,#2653));
#531=EDGE_LOOP('',(#2654,#2655,#2656,#2657,#2658));
#532=EDGE_LOOP('',(#2659,#2660,#2661,#2662,#2663));
#533=EDGE_LOOP('',(#2664,#2665,#2666,#2667,#2668));
#534=EDGE_LOOP('',(#2669));
#535=EDGE_LOOP('',(#2670,#2671,#2672,#2673,#2674));
#536=EDGE_LOOP('',(#2675));
#537=EDGE_LOOP('',(#2676,#2677,#2678));
#538=EDGE_LOOP('',(#2679,#2680,#2681,#2682));
#539=EDGE_LOOP('',(#2683,#2684,#2685));
#540=EDGE_LOOP('',(#2686,#2687,#2688,#2689));
#541=EDGE_LOOP('',(#2690,#2691,#2692,#2693));
#542=EDGE_LOOP('',(#2694,#2695,#2696,#2697));
#543=EDGE_LOOP('',(#2698,#2699,#2700,#2701));
#544=EDGE_LOOP('',(#2702,#2703,#2704,#2705));
#545=EDGE_LOOP('',(#2706,#2707));
#546=EDGE_LOOP('',(#2708,#2709));
#547=EDGE_LOOP('',(#2710,#2711));
#548=EDGE_LOOP('',(#2712,#2713));
#549=EDGE_LOOP('',(#2714,#2715));
#550=EDGE_LOOP('',(#2716,#2717,#2718,#2719));
#551=EDGE_LOOP('',(#2720,#2721));
#552=EDGE_LOOP('',(#2722,#2723));
#553=EDGE_LOOP('',(#2724,#2725));
#554=EDGE_LOOP('',(#2726,#2727,#2728,#2729,#2730));
#555=EDGE_LOOP('',(#2731,#2732,#2733,#2734,#2735,#2736));
#556=EDGE_LOOP('',(#2737,#2738,#2739,#2740,#2741));
#557=EDGE_LOOP('',(#2742));
#558=EDGE_LOOP('',(#2743,#2744,#2745,#2746,#2747));
#559=EDGE_LOOP('',(#2748));
#560=EDGE_LOOP('',(#2749,#2750,#2751,#2752,#2753));
#561=EDGE_LOOP('',(#2754,#2755,#2756,#2757,#2758,#2759,#2760,#2761,#2762,
#2763,#2764,#2765,#2766));
#562=EDGE_LOOP('',(#2767,#2768,#2769,#2770,#2771));
#563=EDGE_LOOP('',(#2772,#2773,#2774,#2775,#2776,#2777,#2778,#2779,#2780,
#2781,#2782,#2783));
#564=EDGE_LOOP('',(#2784,#2785,#2786,#2787,#2788,#2789,#2790,#2791,#2792,
#2793,#2794,#2795,#2796));
#565=EDGE_LOOP('',(#2797,#2798,#2799,#2800,#2801,#2802,#2803,#2804,#2805,
#2806,#2807,#2808));
#566=EDGE_LOOP('',(#2809,#2810,#2811));
#567=EDGE_LOOP('',(#2812,#2813,#2814,#2815));
#568=EDGE_LOOP('',(#2816,#2817,#2818,#2819));
#569=EDGE_LOOP('',(#2820,#2821,#2822,#2823,#2824,#2825,#2826,#2827,#2828,
#2829,#2830,#2831,#2832,#2833));
#570=EDGE_LOOP('',(#2834,#2835,#2836));
#571=EDGE_LOOP('',(#2837,#2838,#2839));
#572=EDGE_LOOP('',(#2840,#2841,#2842));
#573=EDGE_LOOP('',(#2843,#2844,#2845,#2846,#2847,#2848));
#574=EDGE_LOOP('',(#2849,#2850,#2851,#2852,#2853,#2854));
#575=EDGE_LOOP('',(#2855,#2856,#2857));
#576=EDGE_LOOP('',(#2858,#2859,#2860,#2861,#2862,#2863,#2864));
#577=EDGE_LOOP('',(#2865));
#578=EDGE_LOOP('',(#2866,#2867,#2868,#2869,#2870,#2871,#2872));
#579=EDGE_LOOP('',(#2873));
#580=EDGE_LOOP('',(#2874,#2875,#2876,#2877,#2878));
#581=EDGE_LOOP('',(#2879,#2880,#2881,#2882,#2883));
#582=EDGE_LOOP('',(#2884,#2885,#2886,#2887,#2888));
#583=EDGE_LOOP('',(#2889,#2890,#2891,#2892,#2893));
#584=EDGE_LOOP('',(#2894,#2895,#2896,#2897,#2898));
#585=EDGE_LOOP('',(#2899,#2900,#2901,#2902,#2903));
#586=EDGE_LOOP('',(#2904,#2905,#2906));
#587=EDGE_LOOP('',(#2907,#2908,#2909));
#588=EDGE_LOOP('',(#2910,#2911,#2912));
#589=EDGE_LOOP('',(#2913,#2914,#2915));
#590=EDGE_LOOP('',(#2916,#2917,#2918));
#591=EDGE_LOOP('',(#2919,#2920,#2921));
#592=EDGE_LOOP('',(#2922,#2923,#2924,#2925,#2926,#2927));
#593=EDGE_LOOP('',(#2928,#2929,#2930,#2931));
#594=EDGE_LOOP('',(#2932,#2933,#2934,#2935));
#595=EDGE_LOOP('',(#2936,#2937,#2938,#2939));
#596=EDGE_LOOP('',(#2940,#2941,#2942,#2943));
#597=EDGE_LOOP('',(#2944,#2945,#2946,#2947));
#598=EDGE_LOOP('',(#2948,#2949,#2950,#2951));
#599=EDGE_LOOP('',(#2952,#2953,#2954,#2955));
#600=EDGE_LOOP('',(#2956,#2957,#2958,#2959));
#601=EDGE_LOOP('',(#2960,#2961,#2962,#2963));
#602=EDGE_LOOP('',(#2964,#2965,#2966,#2967));
#603=EDGE_LOOP('',(#2968,#2969,#2970,#2971,#2972,#2973,#2974,#2975));
#604=EDGE_LOOP('',(#2976));
#605=EDGE_LOOP('',(#2977,#2978,#2979,#2980,#2981,#2982,#2983,#2984));
#606=EDGE_LOOP('',(#2985));
#607=EDGE_LOOP('',(#2986,#2987,#2988,#2989));
#608=EDGE_LOOP('',(#2990,#2991,#2992,#2993));
#609=EDGE_LOOP('',(#2994,#2995,#2996,#2997));
#610=EDGE_LOOP('',(#2998,#2999,#3000,#3001));
#611=EDGE_LOOP('',(#3002,#3003,#3004,#3005));
#612=EDGE_LOOP('',(#3006,#3007,#3008,#3009));
#613=EDGE_LOOP('',(#3010,#3011,#3012,#3013));
#614=EDGE_LOOP('',(#3014,#3015,#3016,#3017));
#615=EDGE_LOOP('',(#3018,#3019,#3020,#3021));
#616=EDGE_LOOP('',(#3022));
#617=EDGE_LOOP('',(#3023));
#618=EDGE_LOOP('',(#3024));
#619=EDGE_LOOP('',(#3025));
#620=EDGE_LOOP('',(#3026));
#621=EDGE_LOOP('',(#3027));
#622=LINE('',#4656,#925);
#623=LINE('',#4662,#926);
#624=LINE('',#4668,#927);
#625=LINE('',#4674,#928);
#626=LINE('',#4679,#929);
#627=LINE('',#4681,#930);
#628=LINE('',#4683,#931);
#629=LINE('',#4684,#932);
#630=LINE('',#4688,#933);
#631=LINE('',#4690,#934);
#632=LINE('',#4692,#935);
#633=LINE('',#4693,#936);
#634=LINE('',#4697,#937);
#635=LINE('',#4701,#938);
#636=LINE('',#4703,#939);
#637=LINE('',#4705,#940);
#638=LINE('',#4707,#941);
#639=LINE('',#4709,#942);
#640=LINE('',#4713,#943);
#641=LINE('',#4717,#944);
#642=LINE('',#4721,#945);
#643=LINE('',#4725,#946);
#644=LINE('',#4729,#947);
#645=LINE('',#4733,#948);
#646=LINE('',#4737,#949);
#647=LINE('',#4741,#950);
#648=LINE('',#4745,#951);
#649=LINE('',#4747,#952);
#650=LINE('',#4749,#953);
#651=LINE('',#4751,#954);
#652=LINE('',#4753,#955);
#653=LINE('',#4757,#956);
#654=LINE('',#4762,#957);
#655=LINE('',#4764,#958);
#656=LINE('',#4766,#959);
#657=LINE('',#4768,#960);
#658=LINE('',#4770,#961);
#659=LINE('',#4774,#962);
#660=LINE('',#4778,#963);
#661=LINE('',#4782,#964);
#662=LINE('',#4786,#965);
#663=LINE('',#4790,#966);
#664=LINE('',#4794,#967);
#665=LINE('',#4798,#968);
#666=LINE('',#4802,#969);
#667=LINE('',#4806,#970);
#668=LINE('',#4808,#971);
#669=LINE('',#4809,#972);
#670=LINE('',#4811,#973);
#671=LINE('',#4812,#974);
#672=LINE('',#4814,#975);
#673=LINE('',#4815,#976);
#674=LINE('',#4817,#977);
#675=LINE('',#4818,#978);
#676=LINE('',#4820,#979);
#677=LINE('',#4821,#980);
#678=LINE('',#4823,#981);
#679=LINE('',#4824,#982);
#680=LINE('',#4826,#983);
#681=LINE('',#4827,#984);
#682=LINE('',#4829,#985);
#683=LINE('',#4830,#986);
#684=LINE('',#4832,#987);
#685=LINE('',#4833,#988);
#686=LINE('',#4835,#989);
#687=LINE('',#4836,#990);
#688=LINE('',#4838,#991);
#689=LINE('',#4840,#992);
#690=LINE('',#4841,#993);
#691=LINE('',#4844,#994);
#692=LINE('',#4845,#995);
#693=LINE('',#4847,#996);
#694=LINE('',#4848,#997);
#695=LINE('',#4850,#998);
#696=LINE('',#4854,#999);
#697=LINE('',#4856,#1000);
#698=LINE('',#4857,#1001);
#699=LINE('',#4859,#1002);
#700=LINE('',#4860,#1003);
#701=LINE('',#4864,#1004);
#702=LINE('',#4865,#1005);
#703=LINE('',#4866,#1006);
#704=LINE('',#4868,#1007);
#705=LINE('',#4870,#1008);
#706=LINE('',#4871,#1009);
#707=LINE('',#4875,#1010);
#708=LINE('',#4876,#1011);
#709=LINE('',#4877,#1012);
#710=LINE('',#4880,#1013);
#711=LINE('',#4882,#1014);
#712=LINE('',#4884,#1015);
#713=LINE('',#4886,#1016);
#714=LINE('',#4887,#1017);
#715=LINE('',#4888,#1018);
#716=LINE('',#4891,#1019);
#717=LINE('',#4902,#1020);
#718=LINE('',#4903,#1021);
#719=LINE('',#4905,#1022);
#720=LINE('',#4906,#1023);
#721=LINE('',#4912,#1024);
#722=LINE('',#4915,#1025);
#723=LINE('',#4927,#1026);
#724=LINE('',#4933,#1027);
#725=LINE('',#4939,#1028);
#726=LINE('',#4944,#1029);
#727=LINE('',#4948,#1030);
#728=LINE('',#4952,#1031);
#729=LINE('',#4953,#1032);
#730=LINE('',#4956,#1033);
#731=LINE('',#4958,#1034);
#732=LINE('',#4959,#1035);
#733=LINE('',#4963,#1036);
#734=LINE('',#4965,#1037);
#735=LINE('',#4967,#1038);
#736=LINE('',#4969,#1039);
#737=LINE('',#4971,#1040);
#738=LINE('',#4973,#1041);
#739=LINE('',#4975,#1042);
#740=LINE('',#4976,#1043);
#741=LINE('',#4979,#1044);
#742=LINE('',#4981,#1045);
#743=LINE('',#4983,#1046);
#744=LINE('',#4985,#1047);
#745=LINE('',#4989,#1048);
#746=LINE('',#4993,#1049);
#747=LINE('',#4997,#1050);
#748=LINE('',#5001,#1051);
#749=LINE('',#5005,#1052);
#750=LINE('',#5009,#1053);
#751=LINE('',#5013,#1054);
#752=LINE('',#5017,#1055);
#753=LINE('',#5021,#1056);
#754=LINE('',#5023,#1057);
#755=LINE('',#5024,#1058);
#756=LINE('',#5028,#1059);
#757=LINE('',#5032,#1060);
#758=LINE('',#5034,#1061);
#759=LINE('',#5036,#1062);
#760=LINE('',#5041,#1063);
#761=LINE('',#5043,#1064);
#762=LINE('',#5045,#1065);
#763=LINE('',#5046,#1066);
#764=LINE('',#5049,#1067);
#765=LINE('',#5051,#1068);
#766=LINE('',#5053,#1069);
#767=LINE('',#5055,#1070);
#768=LINE('',#5059,#1071);
#769=LINE('',#5063,#1072);
#770=LINE('',#5067,#1073);
#771=LINE('',#5071,#1074);
#772=LINE('',#5075,#1075);
#773=LINE('',#5079,#1076);
#774=LINE('',#5083,#1077);
#775=LINE('',#5087,#1078);
#776=LINE('',#5091,#1079);
#777=LINE('',#5093,#1080);
#778=LINE('',#5094,#1081);
#779=LINE('',#5096,#1082);
#780=LINE('',#5097,#1083);
#781=LINE('',#5099,#1084);
#782=LINE('',#5100,#1085);
#783=LINE('',#5102,#1086);
#784=LINE('',#5103,#1087);
#785=LINE('',#5105,#1088);
#786=LINE('',#5106,#1089);
#787=LINE('',#5108,#1090);
#788=LINE('',#5109,#1091);
#789=LINE('',#5111,#1092);
#790=LINE('',#5112,#1093);
#791=LINE('',#5114,#1094);
#792=LINE('',#5115,#1095);
#793=LINE('',#5117,#1096);
#794=LINE('',#5118,#1097);
#795=LINE('',#5120,#1098);
#796=LINE('',#5121,#1099);
#797=LINE('',#5123,#1100);
#798=LINE('',#5124,#1101);
#799=LINE('',#5125,#1102);
#800=LINE('',#5127,#1103);
#801=LINE('',#5128,#1104);
#802=LINE('',#5132,#1105);
#803=LINE('',#5134,#1106);
#804=LINE('',#5136,#1107);
#805=LINE('',#5138,#1108);
#806=LINE('',#5139,#1109);
#807=LINE('',#5140,#1110);
#808=LINE('',#5141,#1111);
#809=LINE('',#5145,#1112);
#810=LINE('',#5146,#1113);
#811=LINE('',#5147,#1114);
#812=LINE('',#5150,#1115);
#813=LINE('',#5152,#1116);
#814=LINE('',#5154,#1117);
#815=LINE('',#5156,#1118);
#816=LINE('',#5157,#1119);
#817=LINE('',#5158,#1120);
#818=LINE('',#5159,#1121);
#819=LINE('',#5162,#1122);
#820=LINE('',#5173,#1123);
#821=LINE('',#5175,#1124);
#822=LINE('',#5178,#1125);
#823=LINE('',#5180,#1126);
#824=LINE('',#5185,#1127);
#825=LINE('',#5188,#1128);
#826=LINE('',#5200,#1129);
#827=LINE('',#5205,#1130);
#828=LINE('',#5207,#1131);
#829=LINE('',#5209,#1132);
#830=LINE('',#5220,#1133);
#831=LINE('',#5222,#1134);
#832=LINE('',#5224,#1135);
#833=LINE('',#5226,#1136);
#834=LINE('',#5227,#1137);
#835=LINE('',#5231,#1138);
#836=LINE('',#5237,#1139);
#837=LINE('',#5241,#1140);
#838=LINE('',#5244,#1141);
#839=LINE('',#5245,#1142);
#840=LINE('',#5247,#1143);
#841=LINE('',#5251,#1144);
#842=LINE('',#5259,#1145);
#843=LINE('',#5503,#1146);
#844=LINE('',#5505,#1147);
#845=LINE('',#5507,#1148);
#846=LINE('',#5518,#1149);
#847=LINE('',#5520,#1150);
#848=LINE('',#5522,#1151);
#849=LINE('',#5524,#1152);
#850=LINE('',#5526,#1153);
#851=LINE('',#5527,#1154);
#852=LINE('',#5531,#1155);
#853=LINE('',#5537,#1156);
#854=LINE('',#5541,#1157);
#855=LINE('',#5544,#1158);
#856=LINE('',#5545,#1159);
#857=LINE('',#5546,#1160);
#858=LINE('',#5547,#1161);
#859=LINE('',#5548,#1162);
#860=LINE('',#5549,#1163);
#861=LINE('',#5551,#1164);
#862=LINE('',#5571,#1165);
#863=LINE('',#5592,#1166);
#864=LINE('',#5603,#1167);
#865=LINE('',#5622,#1168);
#866=LINE('',#5623,#1169);
#867=LINE('',#5626,#1170);
#868=LINE('',#5627,#1171);
#869=LINE('',#5630,#1172);
#870=LINE('',#5631,#1173);
#871=LINE('',#5635,#1174);
#872=LINE('',#5637,#1175);
#873=LINE('',#5639,#1176);
#874=LINE('',#5641,#1177);
#875=LINE('',#5668,#1178);
#876=LINE('',#5672,#1179);
#877=LINE('',#5674,#1180);
#878=LINE('',#5676,#1181);
#879=LINE('',#5678,#1182);
#880=LINE('',#5705,#1183);
#881=LINE('',#5708,#1184);
#882=LINE('',#5709,#1185);
#883=LINE('',#5720,#1186);
#884=LINE('',#5722,#1187);
#885=LINE('',#5724,#1188);
#886=LINE('',#5726,#1189);
#887=LINE('',#5727,#1190);
#888=LINE('',#5730,#1191);
#889=LINE('',#5731,#1192);
#890=LINE('',#5733,#1193);
#891=LINE('',#5734,#1194);
#892=LINE('',#5737,#1195);
#893=LINE('',#5738,#1196);
#894=LINE('',#5740,#1197);
#895=LINE('',#5741,#1198);
#896=LINE('',#5744,#1199);
#897=LINE('',#5745,#1200);
#898=LINE('',#5747,#1201);
#899=LINE('',#5748,#1202);
#900=LINE('',#5751,#1203);
#901=LINE('',#5752,#1204);
#902=LINE('',#5754,#1205);
#903=LINE('',#5755,#1206);
#904=LINE('',#5757,#1207);
#905=LINE('',#5758,#1208);
#906=LINE('',#5759,#1209);
#907=LINE('',#5889,#1210);
#908=LINE('',#5896,#1211);
#909=LINE('',#5899,#1212);
#910=LINE('',#5905,#1213);
#911=LINE('',#5908,#1214);
#912=LINE('',#5912,#1215);
#913=LINE('',#5916,#1216);
#914=LINE('',#5918,#1217);
#915=LINE('',#5925,#1218);
#916=LINE('',#5927,#1219);
#917=LINE('',#5930,#1220);
#918=LINE('',#5933,#1221);
#919=LINE('',#5934,#1222);
#920=LINE('',#5936,#1223);
#921=LINE('',#5937,#1224);
#922=LINE('',#5946,#1225);
#923=LINE('',#5952,#1226);
#924=LINE('',#5958,#1227);
#925=VECTOR('',#3693,2.);
#926=VECTOR('',#3700,2.);
#927=VECTOR('',#3707,2.);
#928=VECTOR('',#3714,2.);
#929=VECTOR('',#3719,1000.);
#930=VECTOR('',#3720,1000.);
#931=VECTOR('',#3721,1000.);
#932=VECTOR('',#3722,1000.);
#933=VECTOR('',#3725,1000.);
#934=VECTOR('',#3726,1000.);
#935=VECTOR('',#3727,1000.);
#936=VECTOR('',#3728,1000.);
#937=VECTOR('',#3731,1000.);
#938=VECTOR('',#3734,1000.);
#939=VECTOR('',#3735,1000.);
#940=VECTOR('',#3736,1000.);
#941=VECTOR('',#3737,1000.);
#942=VECTOR('',#3738,1000.);
#943=VECTOR('',#3741,1000.);
#944=VECTOR('',#3744,1000.);
#945=VECTOR('',#3747,1000.);
#946=VECTOR('',#3750,1000.);
#947=VECTOR('',#3753,1000.);
#948=VECTOR('',#3756,1000.);
#949=VECTOR('',#3759,1000.);
#950=VECTOR('',#3762,1000.);
#951=VECTOR('',#3765,1000.);
#952=VECTOR('',#3766,1000.);
#953=VECTOR('',#3767,1000.);
#954=VECTOR('',#3768,1000.);
#955=VECTOR('',#3769,1000.);
#956=VECTOR('',#3774,1000.);
#957=VECTOR('',#3779,1000.);
#958=VECTOR('',#3780,1000.);
#959=VECTOR('',#3781,1000.);
#960=VECTOR('',#3782,1000.);
#961=VECTOR('',#3783,1000.);
#962=VECTOR('',#3786,1000.);
#963=VECTOR('',#3789,1000.);
#964=VECTOR('',#3792,1000.);
#965=VECTOR('',#3795,1000.);
#966=VECTOR('',#3798,1000.);
#967=VECTOR('',#3801,1000.);
#968=VECTOR('',#3804,1000.);
#969=VECTOR('',#3807,1000.);
#970=VECTOR('',#3810,1000.);
#971=VECTOR('',#3811,1000.);
#972=VECTOR('',#3812,1000.);
#973=VECTOR('',#3815,1000.);
#974=VECTOR('',#3816,1000.);
#975=VECTOR('',#3819,1000.);
#976=VECTOR('',#3820,1000.);
#977=VECTOR('',#3823,1000.);
#978=VECTOR('',#3824,1000.);
#979=VECTOR('',#3827,1000.);
#980=VECTOR('',#3828,1000.);
#981=VECTOR('',#3831,1000.);
#982=VECTOR('',#3832,1000.);
#983=VECTOR('',#3835,1000.);
#984=VECTOR('',#3836,1000.);
#985=VECTOR('',#3839,1000.);
#986=VECTOR('',#3840,1000.);
#987=VECTOR('',#3843,1000.);
#988=VECTOR('',#3844,1000.);
#989=VECTOR('',#3847,1000.);
#990=VECTOR('',#3848,1000.);
#991=VECTOR('',#3851,1000.);
#992=VECTOR('',#3852,1000.);
#993=VECTOR('',#3853,1000.);
#994=VECTOR('',#3856,1000.);
#995=VECTOR('',#3857,1000.);
#996=VECTOR('',#3860,1000.);
#997=VECTOR('',#3861,1000.);
#998=VECTOR('',#3864,1000.);
#999=VECTOR('',#3867,1000.);
#1000=VECTOR('',#3868,1000.);
#1001=VECTOR('',#3869,1000.);
#1002=VECTOR('',#3870,1000.);
#1003=VECTOR('',#3871,1000.);
#1004=VECTOR('',#3874,1000.);
#1005=VECTOR('',#3875,1000.);
#1006=VECTOR('',#3876,1000.);
#1007=VECTOR('',#3877,1000.);
#1008=VECTOR('',#3878,1000.);
#1009=VECTOR('',#3879,1000.);
#1010=VECTOR('',#3882,1000.);
#1011=VECTOR('',#3883,1000.);
#1012=VECTOR('',#3884,1000.);
#1013=VECTOR('',#3887,1000.);
#1014=VECTOR('',#3888,1000.);
#1015=VECTOR('',#3889,1000.);
#1016=VECTOR('',#3890,1000.);
#1017=VECTOR('',#3891,1000.);
#1018=VECTOR('',#3892,1000.);
#1019=VECTOR('',#3897,1000.);
#1020=VECTOR('',#3918,1000.);
#1021=VECTOR('',#3919,1000.);
#1022=VECTOR('',#3922,1000.);
#1023=VECTOR('',#3923,1000.);
#1024=VECTOR('',#3934,1000.);
#1025=VECTOR('',#3939,1000.);
#1026=VECTOR('',#3958,2.);
#1027=VECTOR('',#3965,2.);
#1028=VECTOR('',#3972,2.);
#1029=VECTOR('',#3977,1000.);
#1030=VECTOR('',#3980,1000.);
#1031=VECTOR('',#3983,1000.);
#1032=VECTOR('',#3984,1000.);
#1033=VECTOR('',#3987,1000.);
#1034=VECTOR('',#3988,1000.);
#1035=VECTOR('',#3989,1000.);
#1036=VECTOR('',#3992,1000.);
#1037=VECTOR('',#3993,1000.);
#1038=VECTOR('',#3994,1000.);
#1039=VECTOR('',#3995,1000.);
#1040=VECTOR('',#3996,1000.);
#1041=VECTOR('',#3997,1000.);
#1042=VECTOR('',#3998,1000.);
#1043=VECTOR('',#3999,1000.);
#1044=VECTOR('',#4002,1000.);
#1045=VECTOR('',#4003,1000.);
#1046=VECTOR('',#4004,1000.);
#1047=VECTOR('',#4005,1000.);
#1048=VECTOR('',#4008,1000.);
#1049=VECTOR('',#4011,1000.);
#1050=VECTOR('',#4014,1000.);
#1051=VECTOR('',#4017,1000.);
#1052=VECTOR('',#4020,1000.);
#1053=VECTOR('',#4023,1000.);
#1054=VECTOR('',#4026,1000.);
#1055=VECTOR('',#4029,1000.);
#1056=VECTOR('',#4032,1000.);
#1057=VECTOR('',#4033,1000.);
#1058=VECTOR('',#4034,1000.);
#1059=VECTOR('',#4037,1000.);
#1060=VECTOR('',#4040,1000.);
#1061=VECTOR('',#4041,1000.);
#1062=VECTOR('',#4042,1000.);
#1063=VECTOR('',#4047,1000.);
#1064=VECTOR('',#4048,1000.);
#1065=VECTOR('',#4049,1000.);
#1066=VECTOR('',#4050,1000.);
#1067=VECTOR('',#4053,1000.);
#1068=VECTOR('',#4054,1000.);
#1069=VECTOR('',#4055,1000.);
#1070=VECTOR('',#4056,1000.);
#1071=VECTOR('',#4059,1000.);
#1072=VECTOR('',#4062,1000.);
#1073=VECTOR('',#4065,1000.);
#1074=VECTOR('',#4068,1000.);
#1075=VECTOR('',#4071,1000.);
#1076=VECTOR('',#4074,1000.);
#1077=VECTOR('',#4077,1000.);
#1078=VECTOR('',#4080,1000.);
#1079=VECTOR('',#4083,1000.);
#1080=VECTOR('',#4084,1000.);
#1081=VECTOR('',#4085,1000.);
#1082=VECTOR('',#4088,1000.);
#1083=VECTOR('',#4089,1000.);
#1084=VECTOR('',#4092,1000.);
#1085=VECTOR('',#4093,1000.);
#1086=VECTOR('',#4096,1000.);
#1087=VECTOR('',#4097,1000.);
#1088=VECTOR('',#4100,1000.);
#1089=VECTOR('',#4101,1000.);
#1090=VECTOR('',#4104,1000.);
#1091=VECTOR('',#4105,1000.);
#1092=VECTOR('',#4108,1000.);
#1093=VECTOR('',#4109,1000.);
#1094=VECTOR('',#4112,1000.);
#1095=VECTOR('',#4113,1000.);
#1096=VECTOR('',#4116,1000.);
#1097=VECTOR('',#4117,1000.);
#1098=VECTOR('',#4120,1000.);
#1099=VECTOR('',#4121,1000.);
#1100=VECTOR('',#4124,1000.);
#1101=VECTOR('',#4125,1000.);
#1102=VECTOR('',#4126,1000.);
#1103=VECTOR('',#4129,1000.);
#1104=VECTOR('',#4130,1000.);
#1105=VECTOR('',#4135,1000.);
#1106=VECTOR('',#4136,1000.);
#1107=VECTOR('',#4137,1000.);
#1108=VECTOR('',#4138,1000.);
#1109=VECTOR('',#4139,1000.);
#1110=VECTOR('',#4140,1000.);
#1111=VECTOR('',#4141,1000.);
#1112=VECTOR('',#4144,1000.);
#1113=VECTOR('',#4145,1000.);
#1114=VECTOR('',#4146,1000.);
#1115=VECTOR('',#4149,1000.);
#1116=VECTOR('',#4150,1000.);
#1117=VECTOR('',#4151,1000.);
#1118=VECTOR('',#4152,1000.);
#1119=VECTOR('',#4153,1000.);
#1120=VECTOR('',#4154,1000.);
#1121=VECTOR('',#4155,1000.);
#1122=VECTOR('',#4160,1000.);
#1123=VECTOR('',#4181,1000.);
#1124=VECTOR('',#4184,1000.);
#1125=VECTOR('',#4189,1000.);
#1126=VECTOR('',#4192,1000.);
#1127=VECTOR('',#4201,1000.);
#1128=VECTOR('',#4206,1000.);
#1129=VECTOR('',#4225,2.);
#1130=VECTOR('',#4230,1000.);
#1131=VECTOR('',#4231,1000.);
#1132=VECTOR('',#4232,1000.);
#1133=VECTOR('',#4235,1000.);
#1134=VECTOR('',#4236,1000.);
#1135=VECTOR('',#4237,1000.);
#1136=VECTOR('',#4238,1000.);
#1137=VECTOR('',#4239,1000.);
#1138=VECTOR('',#4244,1000.);
#1139=VECTOR('',#4253,1000.);
#1140=VECTOR('',#4258,1000.);
#1141=VECTOR('',#4261,1000.);
#1142=VECTOR('',#4262,1000.);
#1143=VECTOR('',#4265,1000.);
#1144=VECTOR('',#4272,1000.);
#1145=VECTOR('',#4283,2.);
#1146=VECTOR('',#4326,1000.);
#1147=VECTOR('',#4327,1000.);
#1148=VECTOR('',#4328,1000.);
#1149=VECTOR('',#4331,1000.);
#1150=VECTOR('',#4332,1000.);
#1151=VECTOR('',#4333,1000.);
#1152=VECTOR('',#4334,1000.);
#1153=VECTOR('',#4335,1000.);
#1154=VECTOR('',#4336,1000.);
#1155=VECTOR('',#4341,1000.);
#1156=VECTOR('',#4350,1000.);
#1157=VECTOR('',#4355,1000.);
#1158=VECTOR('',#4360,1000.);
#1159=VECTOR('',#4361,1000.);
#1160=VECTOR('',#4362,1000.);
#1161=VECTOR('',#4363,1000.);
#1162=VECTOR('',#4364,1000.);
#1163=VECTOR('',#4365,1000.);
#1164=VECTOR('',#4368,1000.);
#1165=VECTOR('',#4381,1000.);
#1166=VECTOR('',#4394,2.);
#1167=VECTOR('',#4405,1.);
#1168=VECTOR('',#4426,1000.);
#1169=VECTOR('',#4427,1000.);
#1170=VECTOR('',#4430,1000.);
#1171=VECTOR('',#4431,1000.);
#1172=VECTOR('',#4434,1000.);
#1173=VECTOR('',#4435,1000.);
#1174=VECTOR('',#4438,1000.);
#1175=VECTOR('',#4439,1000.);
#1176=VECTOR('',#4440,1000.);
#1177=VECTOR('',#4441,1000.);
#1178=VECTOR('',#4442,1000.);
#1179=VECTOR('',#4445,1000.);
#1180=VECTOR('',#4446,1000.);
#1181=VECTOR('',#4447,1000.);
#1182=VECTOR('',#4448,1000.);
#1183=VECTOR('',#4449,1000.);
#1184=VECTOR('',#4452,1000.);
#1185=VECTOR('',#4453,1000.);
#1186=VECTOR('',#4472,1000.);
#1187=VECTOR('',#4473,1000.);
#1188=VECTOR('',#4474,1000.);
#1189=VECTOR('',#4475,1000.);
#1190=VECTOR('',#4476,1000.);
#1191=VECTOR('',#4479,1000.);
#1192=VECTOR('',#4480,1000.);
#1193=VECTOR('',#4481,1000.);
#1194=VECTOR('',#4482,1000.);
#1195=VECTOR('',#4485,1000.);
#1196=VECTOR('',#4486,1000.);
#1197=VECTOR('',#4487,1000.);
#1198=VECTOR('',#4488,1000.);
#1199=VECTOR('',#4491,1000.);
#1200=VECTOR('',#4492,1000.);
#1201=VECTOR('',#4493,1000.);
#1202=VECTOR('',#4494,1000.);
#1203=VECTOR('',#4497,1000.);
#1204=VECTOR('',#4498,1000.);
#1205=VECTOR('',#4499,1000.);
#1206=VECTOR('',#4500,1000.);
#1207=VECTOR('',#4503,1000.);
#1208=VECTOR('',#4504,1000.);
#1209=VECTOR('',#4505,1000.);
#1210=VECTOR('',#4544,2.);
#1211=VECTOR('',#4551,1000.);
#1212=VECTOR('',#4554,1000.);
#1213=VECTOR('',#4559,1000.);
#1214=VECTOR('',#4562,1000.);
#1215=VECTOR('',#4565,1000.);
#1216=VECTOR('',#4568,1000.);
#1217=VECTOR('',#4571,1000.);
#1218=VECTOR('',#4578,1000.);
#1219=VECTOR('',#4581,1000.);
#1220=VECTOR('',#4584,1000.);
#1221=VECTOR('',#4589,1000.);
#1222=VECTOR('',#4590,1000.);
#1223=VECTOR('',#4593,1000.);
#1224=VECTOR('',#4594,1000.);
#1225=VECTOR('',#4607,3.);
#1226=VECTOR('',#4614,3.);
#1227=VECTOR('',#4621,2.);
#1228=CIRCLE('',#3357,2.);
#1229=CIRCLE('',#3358,2.);
#1230=CIRCLE('',#3360,2.);
#1231=CIRCLE('',#3361,2.);
#1232=CIRCLE('',#3363,2.);
#1233=CIRCLE('',#3364,2.);
#1234=CIRCLE('',#3366,2.);
#1235=CIRCLE('',#3367,2.);
#1236=CIRCLE('',#3371,3.5);
#1237=CIRCLE('',#3372,1.);
#1238=CIRCLE('',#3373,1.);
#1239=CIRCLE('',#3374,1.);
#1240=CIRCLE('',#3375,1.);
#1241=CIRCLE('',#3376,1.);
#1242=CIRCLE('',#3377,1.);
#1243=CIRCLE('',#3378,1.);
#1244=CIRCLE('',#3379,1.);
#1245=CIRCLE('',#3380,1.);
#1246=CIRCLE('',#3381,3.5);
#1247=CIRCLE('',#3383,3.5);
#1248=CIRCLE('',#3384,3.5);
#1249=CIRCLE('',#3385,1.);
#1250=CIRCLE('',#3386,1.);
#1251=CIRCLE('',#3387,1.);
#1252=CIRCLE('',#3388,1.);
#1253=CIRCLE('',#3389,1.);
#1254=CIRCLE('',#3390,1.);
#1255=CIRCLE('',#3391,1.);
#1256=CIRCLE('',#3392,1.);
#1257=CIRCLE('',#3393,1.);
#1258=CIRCLE('',#3427,3.5);
#1259=CIRCLE('',#3428,3.5);
#1260=CIRCLE('',#3430,3.5);
#1261=CIRCLE('',#3431,3.5);
#1262=CIRCLE('',#3439,2.);
#1263=CIRCLE('',#3440,2.);
#1264=CIRCLE('',#3442,2.);
#1265=CIRCLE('',#3443,2.);
#1266=CIRCLE('',#3445,2.);
#1267=CIRCLE('',#3446,2.);
#1268=CIRCLE('',#3448,3.5);
#1269=CIRCLE('',#3449,3.5);
#1270=CIRCLE('',#3453,1.);
#1271=CIRCLE('',#3454,1.);
#1272=CIRCLE('',#3455,1.);
#1273=CIRCLE('',#3456,1.);
#1274=CIRCLE('',#3457,1.);
#1275=CIRCLE('',#3458,1.);
#1276=CIRCLE('',#3459,1.);
#1277=CIRCLE('',#3460,1.);
#1278=CIRCLE('',#3461,1.);
#1279=CIRCLE('',#3463,3.5);
#1280=CIRCLE('',#3464,3.5);
#1281=CIRCLE('',#3467,1.);
#1282=CIRCLE('',#3468,1.);
#1283=CIRCLE('',#3469,1.);
#1284=CIRCLE('',#3470,1.);
#1285=CIRCLE('',#3471,1.);
#1286=CIRCLE('',#3472,1.);
#1287=CIRCLE('',#3473,1.);
#1288=CIRCLE('',#3474,1.);
#1289=CIRCLE('',#3475,1.);
#1290=CIRCLE('',#3509,3.5);
#1291=CIRCLE('',#3510,3.5);
#1292=CIRCLE('',#3512,3.5);
#1293=CIRCLE('',#3513,3.5);
#1294=CIRCLE('',#3521,2.);
#1295=CIRCLE('',#3522,2.);
#1296=CIRCLE('',#3526,3.5);
#1297=CIRCLE('',#3527,6.99999999999997);
#1298=CIRCLE('',#3529,3.5);
#1299=CIRCLE('',#3530,6.99999999999997);
#1300=CIRCLE('',#3532,10.);
#1301=CIRCLE('',#3536,10.);
#1302=CIRCLE('',#3542,2.);
#1303=CIRCLE('',#3543,2.);
#1304=CIRCLE('',#3566,3.5);
#1305=CIRCLE('',#3567,6.99999999999997);
#1306=CIRCLE('',#3569,3.5);
#1307=CIRCLE('',#3570,6.99999999999997);
#1308=CIRCLE('',#3572,10.);
#1309=CIRCLE('',#3573,10.);
#1310=CIRCLE('',#3577,10.);
#1311=CIRCLE('',#3578,10.);
#1312=CIRCLE('',#3579,10.);
#1313=CIRCLE('',#3580,10.);
#1314=CIRCLE('',#3587,2.);
#1315=CIRCLE('',#3588,2.);
#1316=CIRCLE('',#3590,1.);
#1317=CIRCLE('',#3591,1.);
#1318=CIRCLE('',#3592,1.);
#1319=CIRCLE('',#3593,1.);
#1320=CIRCLE('',#3594,1.);
#1321=CIRCLE('',#3595,1.);
#1322=CIRCLE('',#3596,1.);
#1323=CIRCLE('',#3597,1.);
#1324=CIRCLE('',#3598,1.);
#1325=CIRCLE('',#3599,1.);
#1326=CIRCLE('',#3600,1.);
#1327=CIRCLE('',#3601,1.);
#1328=CIRCLE('',#3609,3.5);
#1329=CIRCLE('',#3610,3.);
#1330=CIRCLE('',#3611,3.);
#1331=CIRCLE('',#3613,3.5);
#1332=CIRCLE('',#3614,3.);
#1333=CIRCLE('',#3615,3.);
#1334=CIRCLE('',#3630,3.);
#1335=CIRCLE('',#3631,3.);
#1336=CIRCLE('',#3634,3.);
#1337=CIRCLE('',#3635,3.);
#1338=CIRCLE('',#3640,2.);
#1339=CIRCLE('',#3641,2.);
#1340=CIRCLE('',#3643,10.);
#1341=CIRCLE('',#3644,10.);
#1342=CIRCLE('',#3646,5.);
#1343=CIRCLE('',#3647,5.);
#1344=CIRCLE('',#3649,3.5);
#1345=CIRCLE('',#3650,10.);
#1346=CIRCLE('',#3651,10.);
#1347=CIRCLE('',#3653,3.5);
#1348=CIRCLE('',#3654,10.);
#1349=CIRCLE('',#3655,10.);
#1350=CIRCLE('',#3664,3.);
#1351=CIRCLE('',#3665,3.);
#1352=CIRCLE('',#3667,3.);
#1353=CIRCLE('',#3668,3.);
#1354=CIRCLE('',#3670,2.);
#1355=CIRCLE('',#3671,2.);
#1356=VERTEX_POINT('',#4653);
#1357=VERTEX_POINT('',#4655);
#1358=VERTEX_POINT('',#4659);
#1359=VERTEX_POINT('',#4661);
#1360=VERTEX_POINT('',#4665);
#1361=VERTEX_POINT('',#4667);
#1362=VERTEX_POINT('',#4671);
#1363=VERTEX_POINT('',#4673);
#1364=VERTEX_POINT('',#4677);
#1365=VERTEX_POINT('',#4678);
#1366=VERTEX_POINT('',#4680);
#1367=VERTEX_POINT('',#4682);
#1368=VERTEX_POINT('',#4686);
#1369=VERTEX_POINT('',#4687);
#1370=VERTEX_POINT('',#4689);
#1371=VERTEX_POINT('',#4691);
#1372=VERTEX_POINT('',#4695);
#1373=VERTEX_POINT('',#4696);
#1374=VERTEX_POINT('',#4698);
#1375=VERTEX_POINT('',#4700);
#1376=VERTEX_POINT('',#4702);
#1377=VERTEX_POINT('',#4704);
#1378=VERTEX_POINT('',#4706);
#1379=VERTEX_POINT('',#4708);
#1380=VERTEX_POINT('',#4710);
#1381=VERTEX_POINT('',#4712);
#1382=VERTEX_POINT('',#4714);
#1383=VERTEX_POINT('',#4716);
#1384=VERTEX_POINT('',#4718);
#1385=VERTEX_POINT('',#4720);
#1386=VERTEX_POINT('',#4722);
#1387=VERTEX_POINT('',#4724);
#1388=VERTEX_POINT('',#4726);
#1389=VERTEX_POINT('',#4728);
#1390=VERTEX_POINT('',#4730);
#1391=VERTEX_POINT('',#4732);
#1392=VERTEX_POINT('',#4734);
#1393=VERTEX_POINT('',#4736);
#1394=VERTEX_POINT('',#4738);
#1395=VERTEX_POINT('',#4740);
#1396=VERTEX_POINT('',#4742);
#1397=VERTEX_POINT('',#4744);
#1398=VERTEX_POINT('',#4746);
#1399=VERTEX_POINT('',#4748);
#1400=VERTEX_POINT('',#4750);
#1401=VERTEX_POINT('',#4752);
#1402=VERTEX_POINT('',#4756);
#1403=VERTEX_POINT('',#4759);
#1404=VERTEX_POINT('',#4761);
#1405=VERTEX_POINT('',#4763);
#1406=VERTEX_POINT('',#4765);
#1407=VERTEX_POINT('',#4767);
#1408=VERTEX_POINT('',#4769);
#1409=VERTEX_POINT('',#4771);
#1410=VERTEX_POINT('',#4773);
#1411=VERTEX_POINT('',#4775);
#1412=VERTEX_POINT('',#4777);
#1413=VERTEX_POINT('',#4779);
#1414=VERTEX_POINT('',#4781);
#1415=VERTEX_POINT('',#4783);
#1416=VERTEX_POINT('',#4785);
#1417=VERTEX_POINT('',#4787);
#1418=VERTEX_POINT('',#4789);
#1419=VERTEX_POINT('',#4791);
#1420=VERTEX_POINT('',#4793);
#1421=VERTEX_POINT('',#4795);
#1422=VERTEX_POINT('',#4797);
#1423=VERTEX_POINT('',#4799);
#1424=VERTEX_POINT('',#4801);
#1425=VERTEX_POINT('',#4803);
#1426=VERTEX_POINT('',#4805);
#1427=VERTEX_POINT('',#4807);
#1428=VERTEX_POINT('',#4839);
#1429=VERTEX_POINT('',#4843);
#1430=VERTEX_POINT('',#4852);
#1431=VERTEX_POINT('',#4853);
#1432=VERTEX_POINT('',#4855);
#1433=VERTEX_POINT('',#4858);
#1434=VERTEX_POINT('',#4862);
#1435=VERTEX_POINT('',#4863);
#1436=VERTEX_POINT('',#4867);
#1437=VERTEX_POINT('',#4869);
#1438=VERTEX_POINT('',#4873);
#1439=VERTEX_POINT('',#4874);
#1440=VERTEX_POINT('',#4879);
#1441=VERTEX_POINT('',#4881);
#1442=VERTEX_POINT('',#4883);
#1443=VERTEX_POINT('',#4885);
#1444=VERTEX_POINT('',#4924);
#1445=VERTEX_POINT('',#4926);
#1446=VERTEX_POINT('',#4930);
#1447=VERTEX_POINT('',#4932);
#1448=VERTEX_POINT('',#4936);
#1449=VERTEX_POINT('',#4938);
#1450=VERTEX_POINT('',#4942);
#1451=VERTEX_POINT('',#4943);
#1452=VERTEX_POINT('',#4945);
#1453=VERTEX_POINT('',#4947);
#1454=VERTEX_POINT('',#4949);
#1455=VERTEX_POINT('',#4951);
#1456=VERTEX_POINT('',#4955);
#1457=VERTEX_POINT('',#4957);
#1458=VERTEX_POINT('',#4961);
#1459=VERTEX_POINT('',#4962);
#1460=VERTEX_POINT('',#4964);
#1461=VERTEX_POINT('',#4966);
#1462=VERTEX_POINT('',#4968);
#1463=VERTEX_POINT('',#4970);
#1464=VERTEX_POINT('',#4972);
#1465=VERTEX_POINT('',#4974);
#1466=VERTEX_POINT('',#4978);
#1467=VERTEX_POINT('',#4980);
#1468=VERTEX_POINT('',#4982);
#1469=VERTEX_POINT('',#4984);
#1470=VERTEX_POINT('',#4986);
#1471=VERTEX_POINT('',#4988);
#1472=VERTEX_POINT('',#4990);
#1473=VERTEX_POINT('',#4992);
#1474=VERTEX_POINT('',#4994);
#1475=VERTEX_POINT('',#4996);
#1476=VERTEX_POINT('',#4998);
#1477=VERTEX_POINT('',#5000);
#1478=VERTEX_POINT('',#5002);
#1479=VERTEX_POINT('',#5004);
#1480=VERTEX_POINT('',#5006);
#1481=VERTEX_POINT('',#5008);
#1482=VERTEX_POINT('',#5010);
#1483=VERTEX_POINT('',#5012);
#1484=VERTEX_POINT('',#5014);
#1485=VERTEX_POINT('',#5016);
#1486=VERTEX_POINT('',#5018);
#1487=VERTEX_POINT('',#5020);
#1488=VERTEX_POINT('',#5022);
#1489=VERTEX_POINT('',#5026);
#1490=VERTEX_POINT('',#5027);
#1491=VERTEX_POINT('',#5029);
#1492=VERTEX_POINT('',#5031);
#1493=VERTEX_POINT('',#5033);
#1494=VERTEX_POINT('',#5035);
#1495=VERTEX_POINT('',#5039);
#1496=VERTEX_POINT('',#5040);
#1497=VERTEX_POINT('',#5042);
#1498=VERTEX_POINT('',#5044);
#1499=VERTEX_POINT('',#5048);
#1500=VERTEX_POINT('',#5050);
#1501=VERTEX_POINT('',#5052);
#1502=VERTEX_POINT('',#5054);
#1503=VERTEX_POINT('',#5056);
#1504=VERTEX_POINT('',#5058);
#1505=VERTEX_POINT('',#5060);
#1506=VERTEX_POINT('',#5062);
#1507=VERTEX_POINT('',#5064);
#1508=VERTEX_POINT('',#5066);
#1509=VERTEX_POINT('',#5068);
#1510=VERTEX_POINT('',#5070);
#1511=VERTEX_POINT('',#5072);
#1512=VERTEX_POINT('',#5074);
#1513=VERTEX_POINT('',#5076);
#1514=VERTEX_POINT('',#5078);
#1515=VERTEX_POINT('',#5080);
#1516=VERTEX_POINT('',#5082);
#1517=VERTEX_POINT('',#5084);
#1518=VERTEX_POINT('',#5086);
#1519=VERTEX_POINT('',#5088);
#1520=VERTEX_POINT('',#5090);
#1521=VERTEX_POINT('',#5092);
#1522=VERTEX_POINT('',#5131);
#1523=VERTEX_POINT('',#5133);
#1524=VERTEX_POINT('',#5135);
#1525=VERTEX_POINT('',#5137);
#1526=VERTEX_POINT('',#5143);
#1527=VERTEX_POINT('',#5144);
#1528=VERTEX_POINT('',#5149);
#1529=VERTEX_POINT('',#5151);
#1530=VERTEX_POINT('',#5153);
#1531=VERTEX_POINT('',#5155);
#1532=VERTEX_POINT('',#5197);
#1533=VERTEX_POINT('',#5199);
#1534=VERTEX_POINT('',#5203);
#1535=VERTEX_POINT('',#5204);
#1536=VERTEX_POINT('',#5206);
#1537=VERTEX_POINT('',#5208);
#1538=VERTEX_POINT('',#5210);
#1539=VERTEX_POINT('',#5218);
#1540=VERTEX_POINT('',#5219);
#1541=VERTEX_POINT('',#5221);
#1542=VERTEX_POINT('',#5223);
#1543=VERTEX_POINT('',#5225);
#1544=VERTEX_POINT('',#5230);
#1545=VERTEX_POINT('',#5235);
#1546=VERTEX_POINT('',#5239);
#1547=VERTEX_POINT('',#5243);
#1548=VERTEX_POINT('',#5256);
#1549=VERTEX_POINT('',#5258);
#1550=VERTEX_POINT('',#5262);
#1551=VERTEX_POINT('',#5263);
#1552=VERTEX_POINT('',#5301);
#1553=VERTEX_POINT('',#5302);
#1554=VERTEX_POINT('',#5306);
#1555=VERTEX_POINT('',#5307);
#1556=VERTEX_POINT('',#5311);
#1557=VERTEX_POINT('',#5312);
#1558=VERTEX_POINT('',#5316);
#1559=VERTEX_POINT('',#5317);
#1560=VERTEX_POINT('',#5321);
#1561=VERTEX_POINT('',#5322);
#1562=VERTEX_POINT('',#5336);
#1563=VERTEX_POINT('',#5338);
#1564=VERTEX_POINT('',#5354);
#1565=VERTEX_POINT('',#5355);
#1566=VERTEX_POINT('',#5403);
#1567=VERTEX_POINT('',#5404);
#1568=VERTEX_POINT('',#5452);
#1569=VERTEX_POINT('',#5453);
#1570=VERTEX_POINT('',#5501);
#1571=VERTEX_POINT('',#5502);
#1572=VERTEX_POINT('',#5504);
#1573=VERTEX_POINT('',#5506);
#1574=VERTEX_POINT('',#5508);
#1575=VERTEX_POINT('',#5516);
#1576=VERTEX_POINT('',#5517);
#1577=VERTEX_POINT('',#5519);
#1578=VERTEX_POINT('',#5521);
#1579=VERTEX_POINT('',#5523);
#1580=VERTEX_POINT('',#5525);
#1581=VERTEX_POINT('',#5530);
#1582=VERTEX_POINT('',#5535);
#1583=VERTEX_POINT('',#5540);
#1584=VERTEX_POINT('',#5553);
#1585=VERTEX_POINT('',#5589);
#1586=VERTEX_POINT('',#5591);
#1587=VERTEX_POINT('',#5595);
#1588=VERTEX_POINT('',#5596);
#1589=VERTEX_POINT('',#5598);
#1590=VERTEX_POINT('',#5600);
#1591=VERTEX_POINT('',#5602);
#1592=VERTEX_POINT('',#5604);
#1593=VERTEX_POINT('',#5606);
#1594=VERTEX_POINT('',#5608);
#1595=VERTEX_POINT('',#5610);
#1596=VERTEX_POINT('',#5612);
#1597=VERTEX_POINT('',#5615);
#1598=VERTEX_POINT('',#5617);
#1599=VERTEX_POINT('',#5621);
#1600=VERTEX_POINT('',#5625);
#1601=VERTEX_POINT('',#5629);
#1602=VERTEX_POINT('',#5633);
#1603=VERTEX_POINT('',#5634);
#1604=VERTEX_POINT('',#5636);
#1605=VERTEX_POINT('',#5638);
#1606=VERTEX_POINT('',#5640);
#1607=VERTEX_POINT('',#5642);
#1608=VERTEX_POINT('',#5670);
#1609=VERTEX_POINT('',#5671);
#1610=VERTEX_POINT('',#5673);
#1611=VERTEX_POINT('',#5675);
#1612=VERTEX_POINT('',#5677);
#1613=VERTEX_POINT('',#5679);
#1614=VERTEX_POINT('',#5707);
#1615=VERTEX_POINT('',#5719);
#1616=VERTEX_POINT('',#5721);
#1617=VERTEX_POINT('',#5723);
#1618=VERTEX_POINT('',#5725);
#1619=VERTEX_POINT('',#5729);
#1620=VERTEX_POINT('',#5732);
#1621=VERTEX_POINT('',#5736);
#1622=VERTEX_POINT('',#5739);
#1623=VERTEX_POINT('',#5743);
#1624=VERTEX_POINT('',#5746);
#1625=VERTEX_POINT('',#5750);
#1626=VERTEX_POINT('',#5753);
#1627=VERTEX_POINT('',#5886);
#1628=VERTEX_POINT('',#5888);
#1629=VERTEX_POINT('',#5892);
#1630=VERTEX_POINT('',#5893);
#1631=VERTEX_POINT('',#5895);
#1632=VERTEX_POINT('',#5897);
#1633=VERTEX_POINT('',#5901);
#1634=VERTEX_POINT('',#5902);
#1635=VERTEX_POINT('',#5904);
#1636=VERTEX_POINT('',#5906);
#1637=VERTEX_POINT('',#5910);
#1638=VERTEX_POINT('',#5911);
#1639=VERTEX_POINT('',#5913);
#1640=VERTEX_POINT('',#5915);
#1641=VERTEX_POINT('',#5921);
#1642=VERTEX_POINT('',#5922);
#1643=VERTEX_POINT('',#5924);
#1644=VERTEX_POINT('',#5928);
#1645=VERTEX_POINT('',#5943);
#1646=VERTEX_POINT('',#5945);
#1647=VERTEX_POINT('',#5949);
#1648=VERTEX_POINT('',#5951);
#1649=VERTEX_POINT('',#5955);
#1650=VERTEX_POINT('',#5957);
#1651=EDGE_CURVE('',#1356,#1356,#1228,.T.);
#1652=EDGE_CURVE('',#1356,#1357,#622,.T.);
#1653=EDGE_CURVE('',#1357,#1357,#1229,.T.);
#1654=EDGE_CURVE('',#1358,#1358,#1230,.T.);
#1655=EDGE_CURVE('',#1358,#1359,#623,.T.);
#1656=EDGE_CURVE('',#1359,#1359,#1231,.T.);
#1657=EDGE_CURVE('',#1360,#1360,#1232,.T.);
#1658=EDGE_CURVE('',#1360,#1361,#624,.T.);
#1659=EDGE_CURVE('',#1361,#1361,#1233,.T.);
#1660=EDGE_CURVE('',#1362,#1362,#1234,.T.);
#1661=EDGE_CURVE('',#1362,#1363,#625,.T.);
#1662=EDGE_CURVE('',#1363,#1363,#1235,.T.);
#1663=EDGE_CURVE('',#1364,#1365,#626,.T.);
#1664=EDGE_CURVE('',#1365,#1366,#627,.T.);
#1665=EDGE_CURVE('',#1366,#1367,#628,.T.);
#1666=EDGE_CURVE('',#1367,#1364,#629,.T.);
#1667=EDGE_CURVE('',#1368,#1369,#630,.T.);
#1668=EDGE_CURVE('',#1368,#1370,#631,.T.);
#1669=EDGE_CURVE('',#1370,#1371,#632,.T.);
#1670=EDGE_CURVE('',#1369,#1371,#633,.T.);
#1671=EDGE_CURVE('',#1372,#1373,#634,.T.);
#1672=EDGE_CURVE('',#1373,#1374,#1236,.T.);
#1673=EDGE_CURVE('',#1374,#1375,#635,.T.);
#1674=EDGE_CURVE('',#1375,#1376,#636,.T.);
#1675=EDGE_CURVE('',#1376,#1377,#637,.T.);
#1676=EDGE_CURVE('',#1377,#1378,#638,.T.);
#1677=EDGE_CURVE('',#1378,#1379,#639,.T.);
#1678=EDGE_CURVE('',#1380,#1379,#1237,.T.);
#1679=EDGE_CURVE('',#1380,#1381,#640,.T.);
#1680=EDGE_CURVE('',#1382,#1381,#1238,.T.);
#1681=EDGE_CURVE('',#1382,#1383,#641,.T.);
#1682=EDGE_CURVE('',#1384,#1383,#1239,.T.);
#1683=EDGE_CURVE('',#1384,#1385,#642,.T.);
#1684=EDGE_CURVE('',#1386,#1385,#1240,.T.);
#1685=EDGE_CURVE('',#1386,#1387,#643,.T.);
#1686=EDGE_CURVE('',#1388,#1387,#1241,.T.);
#1687=EDGE_CURVE('',#1388,#1389,#644,.T.);
#1688=EDGE_CURVE('',#1390,#1389,#1242,.T.);
#1689=EDGE_CURVE('',#1390,#1391,#645,.T.);
#1690=EDGE_CURVE('',#1392,#1391,#1243,.T.);
#1691=EDGE_CURVE('',#1392,#1393,#646,.T.);
#1692=EDGE_CURVE('',#1394,#1393,#1244,.T.);
#1693=EDGE_CURVE('',#1394,#1395,#647,.T.);
#1694=EDGE_CURVE('',#1396,#1395,#1245,.T.);
#1695=EDGE_CURVE('',#1396,#1397,#648,.T.);
#1696=EDGE_CURVE('',#1397,#1398,#649,.T.);
#1697=EDGE_CURVE('',#1398,#1399,#650,.T.);
#1698=EDGE_CURVE('',#1399,#1400,#651,.T.);
#1699=EDGE_CURVE('',#1400,#1401,#652,.T.);
#1700=EDGE_CURVE('',#1401,#1372,#1246,.T.);
#1701=EDGE_CURVE('',#1402,#1370,#653,.T.);
#1702=EDGE_CURVE('',#1402,#1365,#1247,.T.);
#1703=EDGE_CURVE('',#1364,#1403,#1248,.T.);
#1704=EDGE_CURVE('',#1404,#1403,#654,.T.);
#1705=EDGE_CURVE('',#1405,#1404,#655,.T.);
#1706=EDGE_CURVE('',#1406,#1405,#656,.T.);
#1707=EDGE_CURVE('',#1407,#1406,#657,.T.);
#1708=EDGE_CURVE('',#1408,#1407,#658,.T.);
#1709=EDGE_CURVE('',#1408,#1409,#1249,.T.);
#1710=EDGE_CURVE('',#1410,#1409,#659,.T.);
#1711=EDGE_CURVE('',#1410,#1411,#1250,.T.);
#1712=EDGE_CURVE('',#1412,#1411,#660,.T.);
#1713=EDGE_CURVE('',#1412,#1413,#1251,.T.);
#1714=EDGE_CURVE('',#1414,#1413,#661,.T.);
#1715=EDGE_CURVE('',#1414,#1415,#1252,.T.);
#1716=EDGE_CURVE('',#1416,#1415,#662,.T.);
#1717=EDGE_CURVE('',#1416,#1417,#1253,.T.);
#1718=EDGE_CURVE('',#1418,#1417,#663,.T.);
#1719=EDGE_CURVE('',#1418,#1419,#1254,.T.);
#1720=EDGE_CURVE('',#1420,#1419,#664,.T.);
#1721=EDGE_CURVE('',#1420,#1421,#1255,.T.);
#1722=EDGE_CURVE('',#1422,#1421,#665,.T.);
#1723=EDGE_CURVE('',#1422,#1423,#1256,.T.);
#1724=EDGE_CURVE('',#1424,#1423,#666,.T.);
#1725=EDGE_CURVE('',#1424,#1425,#1257,.T.);
#1726=EDGE_CURVE('',#1426,#1425,#667,.T.);
#1727=EDGE_CURVE('',#1427,#1426,#668,.T.);
#1728=EDGE_CURVE('',#1371,#1427,#669,.T.);
#1729=EDGE_CURVE('',#1411,#1393,#670,.T.);
#1730=EDGE_CURVE('',#1392,#1412,#671,.T.);
#1731=EDGE_CURVE('',#1413,#1391,#672,.T.);
#1732=EDGE_CURVE('',#1390,#1414,#673,.T.);
#1733=EDGE_CURVE('',#1415,#1389,#674,.T.);
#1734=EDGE_CURVE('',#1388,#1416,#675,.T.);
#1735=EDGE_CURVE('',#1417,#1387,#676,.T.);
#1736=EDGE_CURVE('',#1386,#1418,#677,.T.);
#1737=EDGE_CURVE('',#1419,#1385,#678,.T.);
#1738=EDGE_CURVE('',#1384,#1420,#679,.T.);
#1739=EDGE_CURVE('',#1421,#1383,#680,.T.);
#1740=EDGE_CURVE('',#1382,#1422,#681,.T.);
#1741=EDGE_CURVE('',#1423,#1381,#682,.T.);
#1742=EDGE_CURVE('',#1380,#1424,#683,.T.);
#1743=EDGE_CURVE('',#1425,#1379,#684,.T.);
#1744=EDGE_CURVE('',#1378,#1426,#685,.T.);
#1745=EDGE_CURVE('',#1394,#1410,#686,.T.);
#1746=EDGE_CURVE('',#1409,#1395,#687,.T.);
#1747=EDGE_CURVE('',#1377,#1427,#688,.T.);
#1748=EDGE_CURVE('',#1376,#1428,#689,.T.);
#1749=EDGE_CURVE('',#1369,#1428,#690,.T.);
#1750=EDGE_CURVE('',#1375,#1429,#691,.T.);
#1751=EDGE_CURVE('',#1429,#1428,#692,.T.);
#1752=EDGE_CURVE('',#1398,#1406,#693,.T.);
#1753=EDGE_CURVE('',#1397,#1407,#694,.T.);
#1754=EDGE_CURVE('',#1399,#1405,#695,.T.);
#1755=EDGE_CURVE('',#1430,#1431,#696,.T.);
#1756=EDGE_CURVE('',#1431,#1432,#697,.T.);
#1757=EDGE_CURVE('',#1400,#1432,#698,.T.);
#1758=EDGE_CURVE('',#1433,#1404,#699,.T.);
#1759=EDGE_CURVE('',#1430,#1433,#700,.T.);
#1760=EDGE_CURVE('',#1434,#1435,#701,.T.);
#1761=EDGE_CURVE('',#1435,#1401,#702,.T.);
#1762=EDGE_CURVE('',#1433,#1432,#703,.T.);
#1763=EDGE_CURVE('',#1403,#1436,#704,.T.);
#1764=EDGE_CURVE('',#1437,#1436,#705,.T.);
#1765=EDGE_CURVE('',#1434,#1437,#706,.T.);
#1766=EDGE_CURVE('',#1438,#1439,#707,.T.);
#1767=EDGE_CURVE('',#1438,#1373,#708,.T.);
#1768=EDGE_CURVE('',#1372,#1439,#709,.T.);
#1769=EDGE_CURVE('',#1374,#1440,#710,.T.);
#1770=EDGE_CURVE('',#1440,#1441,#711,.T.);
#1771=EDGE_CURVE('',#1442,#1441,#712,.T.);
#1772=EDGE_CURVE('',#1443,#1442,#713,.T.);
#1773=EDGE_CURVE('',#1443,#1402,#714,.T.);
#1774=EDGE_CURVE('',#1368,#1429,#715,.T.);
#1775=EDGE_CURVE('',#1396,#1408,#716,.T.);
#1776=EDGE_CURVE('',#1432,#1429,#717,.T.);
#1777=EDGE_CURVE('',#1433,#1368,#718,.T.);
#1778=EDGE_CURVE('',#1428,#1431,#719,.T.);
#1779=EDGE_CURVE('',#1369,#1430,#720,.T.);
#1780=EDGE_CURVE('',#1440,#1438,#1258,.T.);
#1781=EDGE_CURVE('',#1439,#1435,#1259,.T.);
#1782=EDGE_CURVE('',#1441,#1434,#721,.T.);
#1783=EDGE_CURVE('',#1366,#1443,#1260,.T.);
#1784=EDGE_CURVE('',#1442,#1437,#722,.T.);
#1785=EDGE_CURVE('',#1436,#1367,#1261,.T.);
#1786=EDGE_CURVE('',#1444,#1444,#1262,.T.);
#1787=EDGE_CURVE('',#1444,#1445,#723,.T.);
#1788=EDGE_CURVE('',#1445,#1445,#1263,.T.);
#1789=EDGE_CURVE('',#1446,#1446,#1264,.T.);
#1790=EDGE_CURVE('',#1446,#1447,#724,.T.);
#1791=EDGE_CURVE('',#1447,#1447,#1265,.T.);
#1792=EDGE_CURVE('',#1448,#1448,#1266,.T.);
#1793=EDGE_CURVE('',#1448,#1449,#725,.T.);
#1794=EDGE_CURVE('',#1449,#1449,#1267,.T.);
#1795=EDGE_CURVE('',#1450,#1451,#726,.T.);
#1796=EDGE_CURVE('',#1451,#1452,#1268,.T.);
#1797=EDGE_CURVE('',#1452,#1453,#727,.T.);
#1798=EDGE_CURVE('',#1453,#1454,#1269,.T.);
#1799=EDGE_CURVE('',#1454,#1455,#728,.T.);
#1800=EDGE_CURVE('',#1455,#1450,#729,.T.);
#1801=EDGE_CURVE('',#1452,#1456,#730,.T.);
#1802=EDGE_CURVE('',#1456,#1457,#731,.T.);
#1803=EDGE_CURVE('',#1457,#1453,#732,.T.);
#1804=EDGE_CURVE('',#1458,#1459,#733,.T.);
#1805=EDGE_CURVE('',#1460,#1458,#734,.T.);
#1806=EDGE_CURVE('',#1460,#1461,#735,.T.);
#1807=EDGE_CURVE('',#1461,#1462,#736,.T.);
#1808=EDGE_CURVE('',#1462,#1463,#737,.T.);
#1809=EDGE_CURVE('',#1464,#1463,#738,.T.);
#1810=EDGE_CURVE('',#1465,#1464,#739,.T.);
#1811=EDGE_CURVE('',#1465,#1459,#740,.T.);
#1812=EDGE_CURVE('',#1458,#1466,#741,.T.);
#1813=EDGE_CURVE('',#1466,#1467,#742,.T.);
#1814=EDGE_CURVE('',#1467,#1468,#743,.T.);
#1815=EDGE_CURVE('',#1468,#1469,#744,.T.);
#1816=EDGE_CURVE('',#1470,#1469,#1270,.T.);
#1817=EDGE_CURVE('',#1470,#1471,#745,.T.);
#1818=EDGE_CURVE('',#1472,#1471,#1271,.T.);
#1819=EDGE_CURVE('',#1472,#1473,#746,.T.);
#1820=EDGE_CURVE('',#1474,#1473,#1272,.T.);
#1821=EDGE_CURVE('',#1474,#1475,#747,.T.);
#1822=EDGE_CURVE('',#1476,#1475,#1273,.T.);
#1823=EDGE_CURVE('',#1476,#1477,#748,.T.);
#1824=EDGE_CURVE('',#1478,#1477,#1274,.T.);
#1825=EDGE_CURVE('',#1478,#1479,#749,.T.);
#1826=EDGE_CURVE('',#1480,#1479,#1275,.T.);
#1827=EDGE_CURVE('',#1480,#1481,#750,.T.);
#1828=EDGE_CURVE('',#1482,#1481,#1276,.T.);
#1829=EDGE_CURVE('',#1482,#1483,#751,.T.);
#1830=EDGE_CURVE('',#1484,#1483,#1277,.T.);
#1831=EDGE_CURVE('',#1484,#1485,#752,.T.);
#1832=EDGE_CURVE('',#1486,#1485,#1278,.T.);
#1833=EDGE_CURVE('',#1486,#1487,#753,.T.);
#1834=EDGE_CURVE('',#1487,#1488,#754,.T.);
#1835=EDGE_CURVE('',#1488,#1460,#755,.T.);
#1836=EDGE_CURVE('',#1489,#1490,#756,.T.);
#1837=EDGE_CURVE('',#1489,#1491,#1279,.T.);
#1838=EDGE_CURVE('',#1492,#1491,#757,.T.);
#1839=EDGE_CURVE('',#1493,#1492,#758,.T.);
#1840=EDGE_CURVE('',#1494,#1493,#759,.T.);
#1841=EDGE_CURVE('',#1494,#1490,#1280,.T.);
#1842=EDGE_CURVE('',#1495,#1496,#760,.T.);
#1843=EDGE_CURVE('',#1495,#1497,#761,.T.);
#1844=EDGE_CURVE('',#1497,#1498,#762,.T.);
#1845=EDGE_CURVE('',#1496,#1498,#763,.T.);
#1846=EDGE_CURVE('',#1462,#1499,#764,.T.);
#1847=EDGE_CURVE('',#1500,#1461,#765,.T.);
#1848=EDGE_CURVE('',#1501,#1500,#766,.T.);
#1849=EDGE_CURVE('',#1502,#1501,#767,.T.);
#1850=EDGE_CURVE('',#1502,#1503,#1281,.T.);
#1851=EDGE_CURVE('',#1504,#1503,#768,.T.);
#1852=EDGE_CURVE('',#1504,#1505,#1282,.T.);
#1853=EDGE_CURVE('',#1506,#1505,#769,.T.);
#1854=EDGE_CURVE('',#1506,#1507,#1283,.T.);
#1855=EDGE_CURVE('',#1508,#1507,#770,.T.);
#1856=EDGE_CURVE('',#1508,#1509,#1284,.T.);
#1857=EDGE_CURVE('',#1510,#1509,#771,.T.);
#1858=EDGE_CURVE('',#1510,#1511,#1285,.T.);
#1859=EDGE_CURVE('',#1512,#1511,#772,.T.);
#1860=EDGE_CURVE('',#1512,#1513,#1286,.T.);
#1861=EDGE_CURVE('',#1514,#1513,#773,.T.);
#1862=EDGE_CURVE('',#1514,#1515,#1287,.T.);
#1863=EDGE_CURVE('',#1516,#1515,#774,.T.);
#1864=EDGE_CURVE('',#1516,#1517,#1288,.T.);
#1865=EDGE_CURVE('',#1518,#1517,#775,.T.);
#1866=EDGE_CURVE('',#1518,#1519,#1289,.T.);
#1867=EDGE_CURVE('',#1520,#1519,#776,.T.);
#1868=EDGE_CURVE('',#1521,#1520,#777,.T.);
#1869=EDGE_CURVE('',#1499,#1521,#778,.T.);
#1870=EDGE_CURVE('',#1505,#1483,#779,.T.);
#1871=EDGE_CURVE('',#1482,#1506,#780,.T.);
#1872=EDGE_CURVE('',#1507,#1481,#781,.T.);
#1873=EDGE_CURVE('',#1480,#1508,#782,.T.);
#1874=EDGE_CURVE('',#1509,#1479,#783,.T.);
#1875=EDGE_CURVE('',#1478,#1510,#784,.T.);
#1876=EDGE_CURVE('',#1511,#1477,#785,.T.);
#1877=EDGE_CURVE('',#1476,#1512,#786,.T.);
#1878=EDGE_CURVE('',#1513,#1475,#787,.T.);
#1879=EDGE_CURVE('',#1474,#1514,#788,.T.);
#1880=EDGE_CURVE('',#1515,#1473,#789,.T.);
#1881=EDGE_CURVE('',#1472,#1516,#790,.T.);
#1882=EDGE_CURVE('',#1517,#1471,#791,.T.);
#1883=EDGE_CURVE('',#1470,#1518,#792,.T.);
#1884=EDGE_CURVE('',#1519,#1469,#793,.T.);
#1885=EDGE_CURVE('',#1468,#1520,#794,.T.);
#1886=EDGE_CURVE('',#1484,#1504,#795,.T.);
#1887=EDGE_CURVE('',#1503,#1485,#796,.T.);
#1888=EDGE_CURVE('',#1467,#1521,#797,.T.);
#1889=EDGE_CURVE('',#1466,#1495,#798,.T.);
#1890=EDGE_CURVE('',#1499,#1496,#799,.T.);
#1891=EDGE_CURVE('',#1488,#1500,#800,.T.);
#1892=EDGE_CURVE('',#1487,#1501,#801,.T.);
#1893=EDGE_CURVE('',#1491,#1522,#802,.T.);
#1894=EDGE_CURVE('',#1522,#1523,#803,.T.);
#1895=EDGE_CURVE('',#1524,#1523,#804,.T.);
#1896=EDGE_CURVE('',#1525,#1524,#805,.T.);
#1897=EDGE_CURVE('',#1525,#1451,#806,.T.);
#1898=EDGE_CURVE('',#1450,#1465,#807,.T.);
#1899=EDGE_CURVE('',#1492,#1464,#808,.T.);
#1900=EDGE_CURVE('',#1526,#1527,#809,.T.);
#1901=EDGE_CURVE('',#1526,#1489,#810,.T.);
#1902=EDGE_CURVE('',#1490,#1527,#811,.T.);
#1903=EDGE_CURVE('',#1454,#1528,#812,.T.);
#1904=EDGE_CURVE('',#1528,#1529,#813,.T.);
#1905=EDGE_CURVE('',#1529,#1530,#814,.T.);
#1906=EDGE_CURVE('',#1531,#1530,#815,.T.);
#1907=EDGE_CURVE('',#1531,#1494,#816,.T.);
#1908=EDGE_CURVE('',#1493,#1498,#817,.T.);
#1909=EDGE_CURVE('',#1455,#1497,#818,.T.);
#1910=EDGE_CURVE('',#1486,#1502,#819,.T.);
#1911=EDGE_CURVE('',#1498,#1464,#820,.T.);
#1912=EDGE_CURVE('',#1463,#1496,#821,.T.);
#1913=EDGE_CURVE('',#1497,#1465,#822,.T.);
#1914=EDGE_CURVE('',#1459,#1495,#823,.T.);
#1915=EDGE_CURVE('',#1522,#1526,#1290,.T.);
#1916=EDGE_CURVE('',#1527,#1531,#1291,.T.);
#1917=EDGE_CURVE('',#1523,#1530,#824,.T.);
#1918=EDGE_CURVE('',#1456,#1525,#1292,.T.);
#1919=EDGE_CURVE('',#1524,#1529,#825,.T.);
#1920=EDGE_CURVE('',#1528,#1457,#1293,.T.);
#1921=EDGE_CURVE('',#1532,#1532,#1294,.T.);
#1922=EDGE_CURVE('',#1532,#1533,#826,.T.);
#1923=EDGE_CURVE('',#1533,#1533,#1295,.T.);
#1924=EDGE_CURVE('',#1534,#1535,#827,.T.);
#1925=EDGE_CURVE('',#1534,#1536,#828,.T.);
#1926=EDGE_CURVE('',#1536,#1537,#829,.T.);
#1927=EDGE_CURVE('',#1537,#1538,#81,.T.);
#1928=EDGE_CURVE('',#1538,#1535,#82,.T.);
#1929=EDGE_CURVE('',#1539,#1540,#830,.T.);
#1930=EDGE_CURVE('',#1539,#1541,#831,.T.);
#1931=EDGE_CURVE('',#1541,#1542,#832,.T.);
#1932=EDGE_CURVE('',#1542,#1543,#833,.T.);
#1933=EDGE_CURVE('',#1543,#1540,#834,.T.);
#1934=EDGE_CURVE('',#1541,#1534,#1296,.T.);
#1935=EDGE_CURVE('',#1535,#1544,#835,.T.);
#1936=EDGE_CURVE('',#1544,#1542,#1297,.T.);
#1937=EDGE_CURVE('',#1536,#1539,#1298,.T.);
#1938=EDGE_CURVE('',#1540,#1545,#1299,.T.);
#1939=EDGE_CURVE('',#1545,#1537,#836,.T.);
#1940=EDGE_CURVE('',#1538,#1546,#1300,.T.);
#1941=EDGE_CURVE('',#1546,#1537,#837,.T.);
#1942=EDGE_CURVE('',#1547,#1545,#838,.T.);
#1943=EDGE_CURVE('',#1546,#1547,#839,.T.);
#1944=EDGE_CURVE('',#1535,#1546,#840,.T.);
#1945=EDGE_CURVE('',#1547,#1543,#1301,.T.);
#1946=EDGE_CURVE('',#1544,#1547,#841,.T.);
#1947=EDGE_CURVE('',#1548,#1548,#1302,.T.);
#1948=EDGE_CURVE('',#1548,#1549,#842,.T.);
#1949=EDGE_CURVE('',#1549,#1549,#1303,.T.);
#1950=EDGE_CURVE('',#1550,#1551,#59,.T.);
#1951=EDGE_CURVE('',#1551,#1550,#60,.T.);
#1952=EDGE_CURVE('',#1552,#1553,#49,.T.);
#1953=EDGE_CURVE('',#1553,#1552,#50,.T.);
#1954=EDGE_CURVE('',#1554,#1555,#51,.T.);
#1955=EDGE_CURVE('',#1555,#1554,#52,.T.);
#1956=EDGE_CURVE('',#1556,#1557,#53,.T.);
#1957=EDGE_CURVE('',#1557,#1556,#54,.T.);
#1958=EDGE_CURVE('',#1558,#1559,#55,.T.);
#1959=EDGE_CURVE('',#1559,#1558,#56,.T.);
#1960=EDGE_CURVE('',#1560,#1561,#61,.T.);
#1961=EDGE_CURVE('',#1561,#1562,#57,.T.);
#1962=EDGE_CURVE('',#1562,#1563,#58,.T.);
#1963=EDGE_CURVE('',#1563,#1560,#62,.T.);
#1964=EDGE_CURVE('',#1564,#1565,#63,.T.);
#1965=EDGE_CURVE('',#1565,#1564,#64,.T.);
#1966=EDGE_CURVE('',#1566,#1567,#65,.T.);
#1967=EDGE_CURVE('',#1567,#1566,#66,.T.);
#1968=EDGE_CURVE('',#1568,#1569,#67,.T.);
#1969=EDGE_CURVE('',#1569,#1568,#68,.T.);
#1970=EDGE_CURVE('',#1570,#1571,#843,.T.);
#1971=EDGE_CURVE('',#1570,#1572,#844,.T.);
#1972=EDGE_CURVE('',#1572,#1573,#845,.T.);
#1973=EDGE_CURVE('',#1573,#1574,#83,.T.);
#1974=EDGE_CURVE('',#1574,#1571,#84,.T.);
#1975=EDGE_CURVE('',#1575,#1576,#846,.T.);
#1976=EDGE_CURVE('',#1575,#1577,#847,.T.);
#1977=EDGE_CURVE('',#1577,#1578,#848,.T.);
#1978=EDGE_CURVE('',#1578,#1579,#849,.T.);
#1979=EDGE_CURVE('',#1580,#1579,#850,.T.);
#1980=EDGE_CURVE('',#1580,#1576,#851,.T.);
#1981=EDGE_CURVE('',#1577,#1570,#1304,.T.);
#1982=EDGE_CURVE('',#1571,#1581,#852,.T.);
#1983=EDGE_CURVE('',#1581,#1578,#1305,.T.);
#1984=EDGE_CURVE('',#1572,#1575,#1306,.T.);
#1985=EDGE_CURVE('',#1576,#1582,#1307,.T.);
#1986=EDGE_CURVE('',#1582,#1573,#853,.T.);
#1987=EDGE_CURVE('',#1574,#1551,#1308,.T.);
#1988=EDGE_CURVE('',#1583,#1573,#854,.T.);
#1989=EDGE_CURVE('',#1550,#1583,#1309,.T.);
#1990=EDGE_CURVE('',#1583,#1553,#855,.T.);
#1991=EDGE_CURVE('',#1563,#1582,#856,.T.);
#1992=EDGE_CURVE('',#1558,#1562,#857,.T.);
#1993=EDGE_CURVE('',#1556,#1559,#858,.T.);
#1994=EDGE_CURVE('',#1554,#1557,#859,.T.);
#1995=EDGE_CURVE('',#1552,#1555,#860,.T.);
#1996=EDGE_CURVE('',#1571,#1583,#861,.T.);
#1997=EDGE_CURVE('',#1584,#1580,#69,.T.);
#1998=EDGE_CURVE('',#1564,#1584,#1310,.T.);
#1999=EDGE_CURVE('',#1566,#1565,#1311,.T.);
#2000=EDGE_CURVE('',#1568,#1567,#1312,.T.);
#2001=EDGE_CURVE('',#1560,#1569,#1313,.T.);
#2002=EDGE_CURVE('',#1581,#1561,#862,.T.);
#2003=EDGE_CURVE('',#1579,#1584,#70,.T.);
#2004=EDGE_CURVE('',#1585,#1585,#1314,.T.);
#2005=EDGE_CURVE('',#1585,#1586,#863,.T.);
#2006=EDGE_CURVE('',#1586,#1586,#1315,.T.);
#2007=EDGE_CURVE('',#1587,#1588,#1316,.T.);
#2008=EDGE_CURVE('',#1588,#1589,#1317,.T.);
#2009=EDGE_CURVE('',#1589,#1590,#1318,.T.);
#2010=EDGE_CURVE('',#1590,#1591,#864,.T.);
#2011=EDGE_CURVE('',#1592,#1591,#1319,.T.);
#2012=EDGE_CURVE('',#1593,#1592,#1320,.T.);
#2013=EDGE_CURVE('',#1594,#1593,#1321,.T.);
#2014=EDGE_CURVE('',#1595,#1594,#1322,.T.);
#2015=EDGE_CURVE('',#1596,#1595,#1323,.T.);
#2016=EDGE_CURVE('',#1591,#1596,#1324,.T.);
#2017=EDGE_CURVE('',#1590,#1597,#1325,.T.);
#2018=EDGE_CURVE('',#1597,#1598,#1326,.T.);
#2019=EDGE_CURVE('',#1598,#1587,#1327,.T.);
#2020=EDGE_CURVE('',#1599,#1587,#865,.T.);
#2021=EDGE_CURVE('',#1599,#1588,#866,.T.);
#2022=EDGE_CURVE('',#1590,#1600,#867,.T.);
#2023=EDGE_CURVE('',#1600,#1597,#868,.T.);
#2024=EDGE_CURVE('',#1598,#1601,#869,.T.);
#2025=EDGE_CURVE('',#1587,#1601,#870,.T.);
#2026=EDGE_CURVE('',#1602,#1603,#871,.T.);
#2027=EDGE_CURVE('',#1602,#1604,#872,.T.);
#2028=EDGE_CURVE('',#1604,#1605,#873,.T.);
#2029=EDGE_CURVE('',#1605,#1606,#874,.T.);
#2030=EDGE_CURVE('',#1606,#1607,#71,.T.);
#2031=EDGE_CURVE('',#1607,#1603,#875,.T.);
#2032=EDGE_CURVE('',#1608,#1609,#876,.T.);
#2033=EDGE_CURVE('',#1608,#1610,#877,.T.);
#2034=EDGE_CURVE('',#1610,#1611,#878,.T.);
#2035=EDGE_CURVE('',#1611,#1612,#879,.T.);
#2036=EDGE_CURVE('',#1612,#1613,#72,.T.);
#2037=EDGE_CURVE('',#1613,#1609,#880,.T.);
#2038=EDGE_CURVE('',#1589,#1614,#881,.T.);
#2039=EDGE_CURVE('',#1614,#1590,#882,.T.);
#2040=EDGE_CURVE('',#1604,#1608,#1328,.T.);
#2041=EDGE_CURVE('',#1609,#1599,#1329,.T.);
#2042=EDGE_CURVE('',#1601,#1605,#1330,.T.);
#2043=EDGE_CURVE('',#1610,#1602,#1331,.T.);
#2044=EDGE_CURVE('',#1603,#1600,#1332,.T.);
#2045=EDGE_CURVE('',#1614,#1611,#1333,.T.);
#2046=EDGE_CURVE('',#1615,#1596,#883,.T.);
#2047=EDGE_CURVE('',#1596,#1616,#884,.T.);
#2048=EDGE_CURVE('',#1616,#1617,#885,.T.);
#2049=EDGE_CURVE('',#1618,#1617,#886,.T.);
#2050=EDGE_CURVE('',#1615,#1618,#887,.T.);
#2051=EDGE_CURVE('',#1619,#1591,#888,.T.);
#2052=EDGE_CURVE('',#1591,#1615,#889,.T.);
#2053=EDGE_CURVE('',#1620,#1618,#890,.T.);
#2054=EDGE_CURVE('',#1619,#1620,#891,.T.);
#2055=EDGE_CURVE('',#1621,#1592,#892,.T.);
#2056=EDGE_CURVE('',#1592,#1619,#893,.T.);
#2057=EDGE_CURVE('',#1622,#1620,#894,.T.);
#2058=EDGE_CURVE('',#1621,#1622,#895,.T.);
#2059=EDGE_CURVE('',#1623,#1593,#896,.T.);
#2060=EDGE_CURVE('',#1593,#1621,#897,.T.);
#2061=EDGE_CURVE('',#1624,#1622,#898,.T.);
#2062=EDGE_CURVE('',#1623,#1624,#899,.T.);
#2063=EDGE_CURVE('',#1625,#1594,#900,.T.);
#2064=EDGE_CURVE('',#1594,#1623,#901,.T.);
#2065=EDGE_CURVE('',#1626,#1624,#902,.T.);
#2066=EDGE_CURVE('',#1625,#1626,#903,.T.);
#2067=EDGE_CURVE('',#1616,#1595,#904,.T.);
#2068=EDGE_CURVE('',#1595,#1625,#905,.T.);
#2069=EDGE_CURVE('',#1617,#1626,#906,.T.);
#2070=EDGE_CURVE('',#1597,#1607,#1334,.T.);
#2071=EDGE_CURVE('',#1598,#1606,#1335,.T.);
#2072=EDGE_CURVE('',#1612,#1589,#1336,.T.);
#2073=EDGE_CURVE('',#1613,#1588,#1337,.T.);
#2074=EDGE_CURVE('',#1627,#1627,#1338,.T.);
#2075=EDGE_CURVE('',#1627,#1628,#907,.T.);
#2076=EDGE_CURVE('',#1628,#1628,#1339,.T.);
#2077=EDGE_CURVE('',#1629,#1630,#1340,.T.);
#2078=EDGE_CURVE('',#1629,#1631,#908,.T.);
#2079=EDGE_CURVE('',#1631,#1632,#1341,.T.);
#2080=EDGE_CURVE('',#1630,#1632,#909,.T.);
#2081=EDGE_CURVE('',#1633,#1634,#1342,.T.);
#2082=EDGE_CURVE('',#1633,#1635,#910,.T.);
#2083=EDGE_CURVE('',#1635,#1636,#1343,.T.);
#2084=EDGE_CURVE('',#1636,#1634,#911,.T.);
#2085=EDGE_CURVE('',#1637,#1638,#912,.T.);
#2086=EDGE_CURVE('',#1637,#1639,#1344,.T.);
#2087=EDGE_CURVE('',#1639,#1640,#913,.T.);
#2088=EDGE_CURVE('',#1640,#1629,#1345,.T.);
#2089=EDGE_CURVE('',#1633,#1630,#914,.T.);
#2090=EDGE_CURVE('',#1634,#1638,#1346,.T.);
#2091=EDGE_CURVE('',#1641,#1642,#1347,.T.);
#2092=EDGE_CURVE('',#1642,#1643,#915,.T.);
#2093=EDGE_CURVE('',#1643,#1636,#1348,.T.);
#2094=EDGE_CURVE('',#1632,#1635,#916,.T.);
#2095=EDGE_CURVE('',#1631,#1644,#1349,.T.);
#2096=EDGE_CURVE('',#1641,#1644,#917,.T.);
#2097=EDGE_CURVE('',#1639,#1641,#918,.T.);
#2098=EDGE_CURVE('',#1640,#1644,#919,.T.);
#2099=EDGE_CURVE('',#1642,#1637,#920,.T.);
#2100=EDGE_CURVE('',#1638,#1643,#921,.T.);
#2101=EDGE_CURVE('',#1645,#1645,#1350,.T.);
#2102=EDGE_CURVE('',#1645,#1646,#922,.T.);
#2103=EDGE_CURVE('',#1646,#1646,#1351,.T.);
#2104=EDGE_CURVE('',#1647,#1647,#1352,.T.);
#2105=EDGE_CURVE('',#1647,#1648,#923,.T.);
#2106=EDGE_CURVE('',#1648,#1648,#1353,.T.);
#2107=EDGE_CURVE('',#1649,#1649,#1354,.T.);
#2108=EDGE_CURVE('',#1649,#1650,#924,.T.);
#2109=EDGE_CURVE('',#1650,#1650,#1355,.T.);
#2110=ORIENTED_EDGE('',*,*,#1651,.F.);
#2111=ORIENTED_EDGE('',*,*,#1652,.T.);
#2112=ORIENTED_EDGE('',*,*,#1653,.F.);
#2113=ORIENTED_EDGE('',*,*,#1652,.F.);
#2114=ORIENTED_EDGE('',*,*,#1654,.T.);
#2115=ORIENTED_EDGE('',*,*,#1655,.T.);
#2116=ORIENTED_EDGE('',*,*,#1656,.T.);
#2117=ORIENTED_EDGE('',*,*,#1655,.F.);
#2118=ORIENTED_EDGE('',*,*,#1657,.F.);
#2119=ORIENTED_EDGE('',*,*,#1658,.T.);
#2120=ORIENTED_EDGE('',*,*,#1659,.T.);
#2121=ORIENTED_EDGE('',*,*,#1658,.F.);
#2122=ORIENTED_EDGE('',*,*,#1660,.F.);
#2123=ORIENTED_EDGE('',*,*,#1661,.T.);
#2124=ORIENTED_EDGE('',*,*,#1662,.T.);
#2125=ORIENTED_EDGE('',*,*,#1661,.F.);
#2126=ORIENTED_EDGE('',*,*,#1663,.T.);
#2127=ORIENTED_EDGE('',*,*,#1664,.T.);
#2128=ORIENTED_EDGE('',*,*,#1665,.T.);
#2129=ORIENTED_EDGE('',*,*,#1666,.T.);
#2130=ORIENTED_EDGE('',*,*,#1667,.F.);
#2131=ORIENTED_EDGE('',*,*,#1668,.T.);
#2132=ORIENTED_EDGE('',*,*,#1669,.T.);
#2133=ORIENTED_EDGE('',*,*,#1670,.F.);
#2134=ORIENTED_EDGE('',*,*,#1671,.T.);
#2135=ORIENTED_EDGE('',*,*,#1672,.T.);
#2136=ORIENTED_EDGE('',*,*,#1673,.T.);
#2137=ORIENTED_EDGE('',*,*,#1674,.T.);
#2138=ORIENTED_EDGE('',*,*,#1675,.T.);
#2139=ORIENTED_EDGE('',*,*,#1676,.T.);
#2140=ORIENTED_EDGE('',*,*,#1677,.T.);
#2141=ORIENTED_EDGE('',*,*,#1678,.F.);
#2142=ORIENTED_EDGE('',*,*,#1679,.T.);
#2143=ORIENTED_EDGE('',*,*,#1680,.F.);
#2144=ORIENTED_EDGE('',*,*,#1681,.T.);
#2145=ORIENTED_EDGE('',*,*,#1682,.F.);
#2146=ORIENTED_EDGE('',*,*,#1683,.T.);
#2147=ORIENTED_EDGE('',*,*,#1684,.F.);
#2148=ORIENTED_EDGE('',*,*,#1685,.T.);
#2149=ORIENTED_EDGE('',*,*,#1686,.F.);
#2150=ORIENTED_EDGE('',*,*,#1687,.T.);
#2151=ORIENTED_EDGE('',*,*,#1688,.F.);
#2152=ORIENTED_EDGE('',*,*,#1689,.T.);
#2153=ORIENTED_EDGE('',*,*,#1690,.F.);
#2154=ORIENTED_EDGE('',*,*,#1691,.T.);
#2155=ORIENTED_EDGE('',*,*,#1692,.F.);
#2156=ORIENTED_EDGE('',*,*,#1693,.T.);
#2157=ORIENTED_EDGE('',*,*,#1694,.F.);
#2158=ORIENTED_EDGE('',*,*,#1695,.T.);
#2159=ORIENTED_EDGE('',*,*,#1696,.T.);
#2160=ORIENTED_EDGE('',*,*,#1697,.T.);
#2161=ORIENTED_EDGE('',*,*,#1698,.T.);
#2162=ORIENTED_EDGE('',*,*,#1699,.T.);
#2163=ORIENTED_EDGE('',*,*,#1700,.T.);
#2164=ORIENTED_EDGE('',*,*,#1651,.T.);
#2165=ORIENTED_EDGE('',*,*,#1662,.F.);
#2166=ORIENTED_EDGE('',*,*,#1701,.F.);
#2167=ORIENTED_EDGE('',*,*,#1702,.T.);
#2168=ORIENTED_EDGE('',*,*,#1663,.F.);
#2169=ORIENTED_EDGE('',*,*,#1703,.T.);
#2170=ORIENTED_EDGE('',*,*,#1704,.F.);
#2171=ORIENTED_EDGE('',*,*,#1705,.F.);
#2172=ORIENTED_EDGE('',*,*,#1706,.F.);
#2173=ORIENTED_EDGE('',*,*,#1707,.F.);
#2174=ORIENTED_EDGE('',*,*,#1708,.F.);
#2175=ORIENTED_EDGE('',*,*,#1709,.T.);
#2176=ORIENTED_EDGE('',*,*,#1710,.F.);
#2177=ORIENTED_EDGE('',*,*,#1711,.T.);
#2178=ORIENTED_EDGE('',*,*,#1712,.F.);
#2179=ORIENTED_EDGE('',*,*,#1713,.T.);
#2180=ORIENTED_EDGE('',*,*,#1714,.F.);
#2181=ORIENTED_EDGE('',*,*,#1715,.T.);
#2182=ORIENTED_EDGE('',*,*,#1716,.F.);
#2183=ORIENTED_EDGE('',*,*,#1717,.T.);
#2184=ORIENTED_EDGE('',*,*,#1718,.F.);
#2185=ORIENTED_EDGE('',*,*,#1719,.T.);
#2186=ORIENTED_EDGE('',*,*,#1720,.F.);
#2187=ORIENTED_EDGE('',*,*,#1721,.T.);
#2188=ORIENTED_EDGE('',*,*,#1722,.F.);
#2189=ORIENTED_EDGE('',*,*,#1723,.T.);
#2190=ORIENTED_EDGE('',*,*,#1724,.F.);
#2191=ORIENTED_EDGE('',*,*,#1725,.T.);
#2192=ORIENTED_EDGE('',*,*,#1726,.F.);
#2193=ORIENTED_EDGE('',*,*,#1727,.F.);
#2194=ORIENTED_EDGE('',*,*,#1728,.F.);
#2195=ORIENTED_EDGE('',*,*,#1669,.F.);
#2196=ORIENTED_EDGE('',*,*,#1656,.F.);
#2197=ORIENTED_EDGE('',*,*,#1657,.T.);
#2198=ORIENTED_EDGE('',*,*,#1712,.T.);
#2199=ORIENTED_EDGE('',*,*,#1729,.T.);
#2200=ORIENTED_EDGE('',*,*,#1691,.F.);
#2201=ORIENTED_EDGE('',*,*,#1730,.T.);
#2202=ORIENTED_EDGE('',*,*,#1714,.T.);
#2203=ORIENTED_EDGE('',*,*,#1731,.T.);
#2204=ORIENTED_EDGE('',*,*,#1689,.F.);
#2205=ORIENTED_EDGE('',*,*,#1732,.T.);
#2206=ORIENTED_EDGE('',*,*,#1716,.T.);
#2207=ORIENTED_EDGE('',*,*,#1733,.T.);
#2208=ORIENTED_EDGE('',*,*,#1687,.F.);
#2209=ORIENTED_EDGE('',*,*,#1734,.T.);
#2210=ORIENTED_EDGE('',*,*,#1718,.T.);
#2211=ORIENTED_EDGE('',*,*,#1735,.T.);
#2212=ORIENTED_EDGE('',*,*,#1685,.F.);
#2213=ORIENTED_EDGE('',*,*,#1736,.T.);
#2214=ORIENTED_EDGE('',*,*,#1720,.T.);
#2215=ORIENTED_EDGE('',*,*,#1737,.T.);
#2216=ORIENTED_EDGE('',*,*,#1683,.F.);
#2217=ORIENTED_EDGE('',*,*,#1738,.T.);
#2218=ORIENTED_EDGE('',*,*,#1722,.T.);
#2219=ORIENTED_EDGE('',*,*,#1739,.T.);
#2220=ORIENTED_EDGE('',*,*,#1681,.F.);
#2221=ORIENTED_EDGE('',*,*,#1740,.T.);
#2222=ORIENTED_EDGE('',*,*,#1724,.T.);
#2223=ORIENTED_EDGE('',*,*,#1741,.T.);
#2224=ORIENTED_EDGE('',*,*,#1679,.F.);
#2225=ORIENTED_EDGE('',*,*,#1742,.T.);
#2226=ORIENTED_EDGE('',*,*,#1726,.T.);
#2227=ORIENTED_EDGE('',*,*,#1743,.T.);
#2228=ORIENTED_EDGE('',*,*,#1677,.F.);
#2229=ORIENTED_EDGE('',*,*,#1744,.T.);
#2230=ORIENTED_EDGE('',*,*,#1693,.F.);
#2231=ORIENTED_EDGE('',*,*,#1745,.T.);
#2232=ORIENTED_EDGE('',*,*,#1710,.T.);
#2233=ORIENTED_EDGE('',*,*,#1746,.T.);
#2234=ORIENTED_EDGE('',*,*,#1747,.F.);
#2235=ORIENTED_EDGE('',*,*,#1675,.F.);
#2236=ORIENTED_EDGE('',*,*,#1748,.T.);
#2237=ORIENTED_EDGE('',*,*,#1749,.F.);
#2238=ORIENTED_EDGE('',*,*,#1670,.T.);
#2239=ORIENTED_EDGE('',*,*,#1728,.T.);
#2240=ORIENTED_EDGE('',*,*,#1750,.T.);
#2241=ORIENTED_EDGE('',*,*,#1751,.T.);
#2242=ORIENTED_EDGE('',*,*,#1748,.F.);
#2243=ORIENTED_EDGE('',*,*,#1674,.F.);
#2244=ORIENTED_EDGE('',*,*,#1707,.T.);
#2245=ORIENTED_EDGE('',*,*,#1752,.F.);
#2246=ORIENTED_EDGE('',*,*,#1696,.F.);
#2247=ORIENTED_EDGE('',*,*,#1753,.T.);
#2248=ORIENTED_EDGE('',*,*,#1706,.T.);
#2249=ORIENTED_EDGE('',*,*,#1754,.F.);
#2250=ORIENTED_EDGE('',*,*,#1697,.F.);
#2251=ORIENTED_EDGE('',*,*,#1752,.T.);
#2252=ORIENTED_EDGE('',*,*,#1755,.T.);
#2253=ORIENTED_EDGE('',*,*,#1756,.T.);
#2254=ORIENTED_EDGE('',*,*,#1757,.F.);
#2255=ORIENTED_EDGE('',*,*,#1698,.F.);
#2256=ORIENTED_EDGE('',*,*,#1754,.T.);
#2257=ORIENTED_EDGE('',*,*,#1705,.T.);
#2258=ORIENTED_EDGE('',*,*,#1758,.F.);
#2259=ORIENTED_EDGE('',*,*,#1759,.F.);
#2260=ORIENTED_EDGE('',*,*,#1760,.T.);
#2261=ORIENTED_EDGE('',*,*,#1761,.T.);
#2262=ORIENTED_EDGE('',*,*,#1699,.F.);
#2263=ORIENTED_EDGE('',*,*,#1757,.T.);
#2264=ORIENTED_EDGE('',*,*,#1762,.F.);
#2265=ORIENTED_EDGE('',*,*,#1758,.T.);
#2266=ORIENTED_EDGE('',*,*,#1704,.T.);
#2267=ORIENTED_EDGE('',*,*,#1763,.T.);
#2268=ORIENTED_EDGE('',*,*,#1764,.F.);
#2269=ORIENTED_EDGE('',*,*,#1765,.F.);
#2270=ORIENTED_EDGE('',*,*,#1766,.F.);
#2271=ORIENTED_EDGE('',*,*,#1767,.T.);
#2272=ORIENTED_EDGE('',*,*,#1671,.F.);
#2273=ORIENTED_EDGE('',*,*,#1768,.T.);
#2274=ORIENTED_EDGE('',*,*,#1673,.F.);
#2275=ORIENTED_EDGE('',*,*,#1769,.T.);
#2276=ORIENTED_EDGE('',*,*,#1770,.T.);
#2277=ORIENTED_EDGE('',*,*,#1771,.F.);
#2278=ORIENTED_EDGE('',*,*,#1772,.F.);
#2279=ORIENTED_EDGE('',*,*,#1773,.T.);
#2280=ORIENTED_EDGE('',*,*,#1701,.T.);
#2281=ORIENTED_EDGE('',*,*,#1668,.F.);
#2282=ORIENTED_EDGE('',*,*,#1774,.T.);
#2283=ORIENTED_EDGE('',*,*,#1750,.F.);
#2284=ORIENTED_EDGE('',*,*,#1727,.T.);
#2285=ORIENTED_EDGE('',*,*,#1744,.F.);
#2286=ORIENTED_EDGE('',*,*,#1676,.F.);
#2287=ORIENTED_EDGE('',*,*,#1747,.T.);
#2288=ORIENTED_EDGE('',*,*,#1695,.F.);
#2289=ORIENTED_EDGE('',*,*,#1775,.T.);
#2290=ORIENTED_EDGE('',*,*,#1708,.T.);
#2291=ORIENTED_EDGE('',*,*,#1753,.F.);
#2292=ORIENTED_EDGE('',*,*,#1709,.F.);
#2293=ORIENTED_EDGE('',*,*,#1775,.F.);
#2294=ORIENTED_EDGE('',*,*,#1694,.T.);
#2295=ORIENTED_EDGE('',*,*,#1746,.F.);
#2296=ORIENTED_EDGE('',*,*,#1725,.F.);
#2297=ORIENTED_EDGE('',*,*,#1742,.F.);
#2298=ORIENTED_EDGE('',*,*,#1678,.T.);
#2299=ORIENTED_EDGE('',*,*,#1743,.F.);
#2300=ORIENTED_EDGE('',*,*,#1723,.F.);
#2301=ORIENTED_EDGE('',*,*,#1740,.F.);
#2302=ORIENTED_EDGE('',*,*,#1680,.T.);
#2303=ORIENTED_EDGE('',*,*,#1741,.F.);
#2304=ORIENTED_EDGE('',*,*,#1721,.F.);
#2305=ORIENTED_EDGE('',*,*,#1738,.F.);
#2306=ORIENTED_EDGE('',*,*,#1682,.T.);
#2307=ORIENTED_EDGE('',*,*,#1739,.F.);
#2308=ORIENTED_EDGE('',*,*,#1719,.F.);
#2309=ORIENTED_EDGE('',*,*,#1736,.F.);
#2310=ORIENTED_EDGE('',*,*,#1684,.T.);
#2311=ORIENTED_EDGE('',*,*,#1737,.F.);
#2312=ORIENTED_EDGE('',*,*,#1717,.F.);
#2313=ORIENTED_EDGE('',*,*,#1734,.F.);
#2314=ORIENTED_EDGE('',*,*,#1686,.T.);
#2315=ORIENTED_EDGE('',*,*,#1735,.F.);
#2316=ORIENTED_EDGE('',*,*,#1715,.F.);
#2317=ORIENTED_EDGE('',*,*,#1732,.F.);
#2318=ORIENTED_EDGE('',*,*,#1688,.T.);
#2319=ORIENTED_EDGE('',*,*,#1733,.F.);
#2320=ORIENTED_EDGE('',*,*,#1713,.F.);
#2321=ORIENTED_EDGE('',*,*,#1730,.F.);
#2322=ORIENTED_EDGE('',*,*,#1690,.T.);
#2323=ORIENTED_EDGE('',*,*,#1731,.F.);
#2324=ORIENTED_EDGE('',*,*,#1711,.F.);
#2325=ORIENTED_EDGE('',*,*,#1745,.F.);
#2326=ORIENTED_EDGE('',*,*,#1692,.T.);
#2327=ORIENTED_EDGE('',*,*,#1729,.F.);
#2328=ORIENTED_EDGE('',*,*,#1776,.T.);
#2329=ORIENTED_EDGE('',*,*,#1774,.F.);
#2330=ORIENTED_EDGE('',*,*,#1777,.F.);
#2331=ORIENTED_EDGE('',*,*,#1762,.T.);
#2332=ORIENTED_EDGE('',*,*,#1778,.T.);
#2333=ORIENTED_EDGE('',*,*,#1755,.F.);
#2334=ORIENTED_EDGE('',*,*,#1779,.F.);
#2335=ORIENTED_EDGE('',*,*,#1749,.T.);
#2336=ORIENTED_EDGE('',*,*,#1667,.T.);
#2337=ORIENTED_EDGE('',*,*,#1779,.T.);
#2338=ORIENTED_EDGE('',*,*,#1759,.T.);
#2339=ORIENTED_EDGE('',*,*,#1777,.T.);
#2340=ORIENTED_EDGE('',*,*,#1659,.F.);
#2341=ORIENTED_EDGE('',*,*,#1751,.F.);
#2342=ORIENTED_EDGE('',*,*,#1776,.F.);
#2343=ORIENTED_EDGE('',*,*,#1756,.F.);
#2344=ORIENTED_EDGE('',*,*,#1778,.F.);
#2345=ORIENTED_EDGE('',*,*,#1660,.T.);
#2346=ORIENTED_EDGE('',*,*,#1770,.F.);
#2347=ORIENTED_EDGE('',*,*,#1780,.T.);
#2348=ORIENTED_EDGE('',*,*,#1766,.T.);
#2349=ORIENTED_EDGE('',*,*,#1781,.T.);
#2350=ORIENTED_EDGE('',*,*,#1760,.F.);
#2351=ORIENTED_EDGE('',*,*,#1782,.F.);
#2352=ORIENTED_EDGE('',*,*,#1653,.T.);
#2353=ORIENTED_EDGE('',*,*,#1665,.F.);
#2354=ORIENTED_EDGE('',*,*,#1783,.T.);
#2355=ORIENTED_EDGE('',*,*,#1772,.T.);
#2356=ORIENTED_EDGE('',*,*,#1784,.T.);
#2357=ORIENTED_EDGE('',*,*,#1764,.T.);
#2358=ORIENTED_EDGE('',*,*,#1785,.T.);
#2359=ORIENTED_EDGE('',*,*,#1654,.F.);
#2360=ORIENTED_EDGE('',*,*,#1765,.T.);
#2361=ORIENTED_EDGE('',*,*,#1784,.F.);
#2362=ORIENTED_EDGE('',*,*,#1771,.T.);
#2363=ORIENTED_EDGE('',*,*,#1782,.T.);
#2364=ORIENTED_EDGE('',*,*,#1672,.F.);
#2365=ORIENTED_EDGE('',*,*,#1767,.F.);
#2366=ORIENTED_EDGE('',*,*,#1780,.F.);
#2367=ORIENTED_EDGE('',*,*,#1769,.F.);
#2368=ORIENTED_EDGE('',*,*,#1783,.F.);
#2369=ORIENTED_EDGE('',*,*,#1664,.F.);
#2370=ORIENTED_EDGE('',*,*,#1702,.F.);
#2371=ORIENTED_EDGE('',*,*,#1773,.F.);
#2372=ORIENTED_EDGE('',*,*,#1700,.F.);
#2373=ORIENTED_EDGE('',*,*,#1761,.F.);
#2374=ORIENTED_EDGE('',*,*,#1781,.F.);
#2375=ORIENTED_EDGE('',*,*,#1768,.F.);
#2376=ORIENTED_EDGE('',*,*,#1785,.F.);
#2377=ORIENTED_EDGE('',*,*,#1763,.F.);
#2378=ORIENTED_EDGE('',*,*,#1703,.F.);
#2379=ORIENTED_EDGE('',*,*,#1666,.F.);
#2380=ORIENTED_EDGE('',*,*,#1786,.F.);
#2381=ORIENTED_EDGE('',*,*,#1787,.T.);
#2382=ORIENTED_EDGE('',*,*,#1788,.F.);
#2383=ORIENTED_EDGE('',*,*,#1787,.F.);
#2384=ORIENTED_EDGE('',*,*,#1789,.T.);
#2385=ORIENTED_EDGE('',*,*,#1790,.T.);
#2386=ORIENTED_EDGE('',*,*,#1791,.T.);
#2387=ORIENTED_EDGE('',*,*,#1790,.F.);
#2388=ORIENTED_EDGE('',*,*,#1792,.F.);
#2389=ORIENTED_EDGE('',*,*,#1793,.T.);
#2390=ORIENTED_EDGE('',*,*,#1794,.F.);
#2391=ORIENTED_EDGE('',*,*,#1793,.F.);
#2392=ORIENTED_EDGE('',*,*,#1795,.T.);
#2393=ORIENTED_EDGE('',*,*,#1796,.T.);
#2394=ORIENTED_EDGE('',*,*,#1797,.T.);
#2395=ORIENTED_EDGE('',*,*,#1798,.T.);
#2396=ORIENTED_EDGE('',*,*,#1799,.T.);
#2397=ORIENTED_EDGE('',*,*,#1800,.T.);
#2398=ORIENTED_EDGE('',*,*,#1791,.F.);
#2399=ORIENTED_EDGE('',*,*,#1797,.F.);
#2400=ORIENTED_EDGE('',*,*,#1801,.T.);
#2401=ORIENTED_EDGE('',*,*,#1802,.T.);
#2402=ORIENTED_EDGE('',*,*,#1803,.T.);
#2403=ORIENTED_EDGE('',*,*,#1804,.F.);
#2404=ORIENTED_EDGE('',*,*,#1805,.F.);
#2405=ORIENTED_EDGE('',*,*,#1806,.T.);
#2406=ORIENTED_EDGE('',*,*,#1807,.T.);
#2407=ORIENTED_EDGE('',*,*,#1808,.T.);
#2408=ORIENTED_EDGE('',*,*,#1809,.F.);
#2409=ORIENTED_EDGE('',*,*,#1810,.F.);
#2410=ORIENTED_EDGE('',*,*,#1811,.T.);
#2411=ORIENTED_EDGE('',*,*,#1812,.T.);
#2412=ORIENTED_EDGE('',*,*,#1813,.T.);
#2413=ORIENTED_EDGE('',*,*,#1814,.T.);
#2414=ORIENTED_EDGE('',*,*,#1815,.T.);
#2415=ORIENTED_EDGE('',*,*,#1816,.F.);
#2416=ORIENTED_EDGE('',*,*,#1817,.T.);
#2417=ORIENTED_EDGE('',*,*,#1818,.F.);
#2418=ORIENTED_EDGE('',*,*,#1819,.T.);
#2419=ORIENTED_EDGE('',*,*,#1820,.F.);
#2420=ORIENTED_EDGE('',*,*,#1821,.T.);
#2421=ORIENTED_EDGE('',*,*,#1822,.F.);
#2422=ORIENTED_EDGE('',*,*,#1823,.T.);
#2423=ORIENTED_EDGE('',*,*,#1824,.F.);
#2424=ORIENTED_EDGE('',*,*,#1825,.T.);
#2425=ORIENTED_EDGE('',*,*,#1826,.F.);
#2426=ORIENTED_EDGE('',*,*,#1827,.T.);
#2427=ORIENTED_EDGE('',*,*,#1828,.F.);
#2428=ORIENTED_EDGE('',*,*,#1829,.T.);
#2429=ORIENTED_EDGE('',*,*,#1830,.F.);
#2430=ORIENTED_EDGE('',*,*,#1831,.T.);
#2431=ORIENTED_EDGE('',*,*,#1832,.F.);
#2432=ORIENTED_EDGE('',*,*,#1833,.T.);
#2433=ORIENTED_EDGE('',*,*,#1834,.T.);
#2434=ORIENTED_EDGE('',*,*,#1835,.T.);
#2435=ORIENTED_EDGE('',*,*,#1805,.T.);
#2436=ORIENTED_EDGE('',*,*,#1836,.F.);
#2437=ORIENTED_EDGE('',*,*,#1837,.T.);
#2438=ORIENTED_EDGE('',*,*,#1838,.F.);
#2439=ORIENTED_EDGE('',*,*,#1839,.F.);
#2440=ORIENTED_EDGE('',*,*,#1840,.F.);
#2441=ORIENTED_EDGE('',*,*,#1841,.T.);
#2442=ORIENTED_EDGE('',*,*,#1786,.T.);
#2443=ORIENTED_EDGE('',*,*,#1842,.F.);
#2444=ORIENTED_EDGE('',*,*,#1843,.T.);
#2445=ORIENTED_EDGE('',*,*,#1844,.T.);
#2446=ORIENTED_EDGE('',*,*,#1845,.F.);
#2447=ORIENTED_EDGE('',*,*,#1846,.F.);
#2448=ORIENTED_EDGE('',*,*,#1807,.F.);
#2449=ORIENTED_EDGE('',*,*,#1847,.F.);
#2450=ORIENTED_EDGE('',*,*,#1848,.F.);
#2451=ORIENTED_EDGE('',*,*,#1849,.F.);
#2452=ORIENTED_EDGE('',*,*,#1850,.T.);
#2453=ORIENTED_EDGE('',*,*,#1851,.F.);
#2454=ORIENTED_EDGE('',*,*,#1852,.T.);
#2455=ORIENTED_EDGE('',*,*,#1853,.F.);
#2456=ORIENTED_EDGE('',*,*,#1854,.T.);
#2457=ORIENTED_EDGE('',*,*,#1855,.F.);
#2458=ORIENTED_EDGE('',*,*,#1856,.T.);
#2459=ORIENTED_EDGE('',*,*,#1857,.F.);
#2460=ORIENTED_EDGE('',*,*,#1858,.T.);
#2461=ORIENTED_EDGE('',*,*,#1859,.F.);
#2462=ORIENTED_EDGE('',*,*,#1860,.T.);
#2463=ORIENTED_EDGE('',*,*,#1861,.F.);
#2464=ORIENTED_EDGE('',*,*,#1862,.T.);
#2465=ORIENTED_EDGE('',*,*,#1863,.F.);
#2466=ORIENTED_EDGE('',*,*,#1864,.T.);
#2467=ORIENTED_EDGE('',*,*,#1865,.F.);
#2468=ORIENTED_EDGE('',*,*,#1866,.T.);
#2469=ORIENTED_EDGE('',*,*,#1867,.F.);
#2470=ORIENTED_EDGE('',*,*,#1868,.F.);
#2471=ORIENTED_EDGE('',*,*,#1869,.F.);
#2472=ORIENTED_EDGE('',*,*,#1853,.T.);
#2473=ORIENTED_EDGE('',*,*,#1870,.T.);
#2474=ORIENTED_EDGE('',*,*,#1829,.F.);
#2475=ORIENTED_EDGE('',*,*,#1871,.T.);
#2476=ORIENTED_EDGE('',*,*,#1855,.T.);
#2477=ORIENTED_EDGE('',*,*,#1872,.T.);
#2478=ORIENTED_EDGE('',*,*,#1827,.F.);
#2479=ORIENTED_EDGE('',*,*,#1873,.T.);
#2480=ORIENTED_EDGE('',*,*,#1857,.T.);
#2481=ORIENTED_EDGE('',*,*,#1874,.T.);
#2482=ORIENTED_EDGE('',*,*,#1825,.F.);
#2483=ORIENTED_EDGE('',*,*,#1875,.T.);
#2484=ORIENTED_EDGE('',*,*,#1859,.T.);
#2485=ORIENTED_EDGE('',*,*,#1876,.T.);
#2486=ORIENTED_EDGE('',*,*,#1823,.F.);
#2487=ORIENTED_EDGE('',*,*,#1877,.T.);
#2488=ORIENTED_EDGE('',*,*,#1861,.T.);
#2489=ORIENTED_EDGE('',*,*,#1878,.T.);
#2490=ORIENTED_EDGE('',*,*,#1821,.F.);
#2491=ORIENTED_EDGE('',*,*,#1879,.T.);
#2492=ORIENTED_EDGE('',*,*,#1863,.T.);
#2493=ORIENTED_EDGE('',*,*,#1880,.T.);
#2494=ORIENTED_EDGE('',*,*,#1819,.F.);
#2495=ORIENTED_EDGE('',*,*,#1881,.T.);
#2496=ORIENTED_EDGE('',*,*,#1865,.T.);
#2497=ORIENTED_EDGE('',*,*,#1882,.T.);
#2498=ORIENTED_EDGE('',*,*,#1817,.F.);
#2499=ORIENTED_EDGE('',*,*,#1883,.T.);
#2500=ORIENTED_EDGE('',*,*,#1867,.T.);
#2501=ORIENTED_EDGE('',*,*,#1884,.T.);
#2502=ORIENTED_EDGE('',*,*,#1815,.F.);
#2503=ORIENTED_EDGE('',*,*,#1885,.T.);
#2504=ORIENTED_EDGE('',*,*,#1831,.F.);
#2505=ORIENTED_EDGE('',*,*,#1886,.T.);
#2506=ORIENTED_EDGE('',*,*,#1851,.T.);
#2507=ORIENTED_EDGE('',*,*,#1887,.T.);
#2508=ORIENTED_EDGE('',*,*,#1888,.F.);
#2509=ORIENTED_EDGE('',*,*,#1813,.F.);
#2510=ORIENTED_EDGE('',*,*,#1889,.T.);
#2511=ORIENTED_EDGE('',*,*,#1842,.T.);
#2512=ORIENTED_EDGE('',*,*,#1890,.F.);
#2513=ORIENTED_EDGE('',*,*,#1869,.T.);
#2514=ORIENTED_EDGE('',*,*,#1848,.T.);
#2515=ORIENTED_EDGE('',*,*,#1891,.F.);
#2516=ORIENTED_EDGE('',*,*,#1834,.F.);
#2517=ORIENTED_EDGE('',*,*,#1892,.T.);
#2518=ORIENTED_EDGE('',*,*,#1847,.T.);
#2519=ORIENTED_EDGE('',*,*,#1806,.F.);
#2520=ORIENTED_EDGE('',*,*,#1835,.F.);
#2521=ORIENTED_EDGE('',*,*,#1891,.T.);
#2522=ORIENTED_EDGE('',*,*,#1838,.T.);
#2523=ORIENTED_EDGE('',*,*,#1893,.T.);
#2524=ORIENTED_EDGE('',*,*,#1894,.T.);
#2525=ORIENTED_EDGE('',*,*,#1895,.F.);
#2526=ORIENTED_EDGE('',*,*,#1896,.F.);
#2527=ORIENTED_EDGE('',*,*,#1897,.T.);
#2528=ORIENTED_EDGE('',*,*,#1795,.F.);
#2529=ORIENTED_EDGE('',*,*,#1898,.T.);
#2530=ORIENTED_EDGE('',*,*,#1810,.T.);
#2531=ORIENTED_EDGE('',*,*,#1899,.F.);
#2532=ORIENTED_EDGE('',*,*,#1900,.F.);
#2533=ORIENTED_EDGE('',*,*,#1901,.T.);
#2534=ORIENTED_EDGE('',*,*,#1836,.T.);
#2535=ORIENTED_EDGE('',*,*,#1902,.T.);
#2536=ORIENTED_EDGE('',*,*,#1799,.F.);
#2537=ORIENTED_EDGE('',*,*,#1903,.T.);
#2538=ORIENTED_EDGE('',*,*,#1904,.T.);
#2539=ORIENTED_EDGE('',*,*,#1905,.T.);
#2540=ORIENTED_EDGE('',*,*,#1906,.F.);
#2541=ORIENTED_EDGE('',*,*,#1907,.T.);
#2542=ORIENTED_EDGE('',*,*,#1840,.T.);
#2543=ORIENTED_EDGE('',*,*,#1908,.T.);
#2544=ORIENTED_EDGE('',*,*,#1844,.F.);
#2545=ORIENTED_EDGE('',*,*,#1909,.F.);
#2546=ORIENTED_EDGE('',*,*,#1868,.T.);
#2547=ORIENTED_EDGE('',*,*,#1885,.F.);
#2548=ORIENTED_EDGE('',*,*,#1814,.F.);
#2549=ORIENTED_EDGE('',*,*,#1888,.T.);
#2550=ORIENTED_EDGE('',*,*,#1833,.F.);
#2551=ORIENTED_EDGE('',*,*,#1910,.T.);
#2552=ORIENTED_EDGE('',*,*,#1849,.T.);
#2553=ORIENTED_EDGE('',*,*,#1892,.F.);
#2554=ORIENTED_EDGE('',*,*,#1850,.F.);
#2555=ORIENTED_EDGE('',*,*,#1910,.F.);
#2556=ORIENTED_EDGE('',*,*,#1832,.T.);
#2557=ORIENTED_EDGE('',*,*,#1887,.F.);
#2558=ORIENTED_EDGE('',*,*,#1866,.F.);
#2559=ORIENTED_EDGE('',*,*,#1883,.F.);
#2560=ORIENTED_EDGE('',*,*,#1816,.T.);
#2561=ORIENTED_EDGE('',*,*,#1884,.F.);
#2562=ORIENTED_EDGE('',*,*,#1864,.F.);
#2563=ORIENTED_EDGE('',*,*,#1881,.F.);
#2564=ORIENTED_EDGE('',*,*,#1818,.T.);
#2565=ORIENTED_EDGE('',*,*,#1882,.F.);
#2566=ORIENTED_EDGE('',*,*,#1862,.F.);
#2567=ORIENTED_EDGE('',*,*,#1879,.F.);
#2568=ORIENTED_EDGE('',*,*,#1820,.T.);
#2569=ORIENTED_EDGE('',*,*,#1880,.F.);
#2570=ORIENTED_EDGE('',*,*,#1860,.F.);
#2571=ORIENTED_EDGE('',*,*,#1877,.F.);
#2572=ORIENTED_EDGE('',*,*,#1822,.T.);
#2573=ORIENTED_EDGE('',*,*,#1878,.F.);
#2574=ORIENTED_EDGE('',*,*,#1858,.F.);
#2575=ORIENTED_EDGE('',*,*,#1875,.F.);
#2576=ORIENTED_EDGE('',*,*,#1824,.T.);
#2577=ORIENTED_EDGE('',*,*,#1876,.F.);
#2578=ORIENTED_EDGE('',*,*,#1856,.F.);
#2579=ORIENTED_EDGE('',*,*,#1873,.F.);
#2580=ORIENTED_EDGE('',*,*,#1826,.T.);
#2581=ORIENTED_EDGE('',*,*,#1874,.F.);
#2582=ORIENTED_EDGE('',*,*,#1854,.F.);
#2583=ORIENTED_EDGE('',*,*,#1871,.F.);
#2584=ORIENTED_EDGE('',*,*,#1828,.T.);
#2585=ORIENTED_EDGE('',*,*,#1872,.F.);
#2586=ORIENTED_EDGE('',*,*,#1852,.F.);
#2587=ORIENTED_EDGE('',*,*,#1886,.F.);
#2588=ORIENTED_EDGE('',*,*,#1830,.T.);
#2589=ORIENTED_EDGE('',*,*,#1870,.F.);
#2590=ORIENTED_EDGE('',*,*,#1908,.F.);
#2591=ORIENTED_EDGE('',*,*,#1839,.T.);
#2592=ORIENTED_EDGE('',*,*,#1899,.T.);
#2593=ORIENTED_EDGE('',*,*,#1911,.F.);
#2594=ORIENTED_EDGE('',*,*,#1808,.F.);
#2595=ORIENTED_EDGE('',*,*,#1846,.T.);
#2596=ORIENTED_EDGE('',*,*,#1890,.T.);
#2597=ORIENTED_EDGE('',*,*,#1912,.F.);
#2598=ORIENTED_EDGE('',*,*,#1845,.T.);
#2599=ORIENTED_EDGE('',*,*,#1911,.T.);
#2600=ORIENTED_EDGE('',*,*,#1809,.T.);
#2601=ORIENTED_EDGE('',*,*,#1912,.T.);
#2602=ORIENTED_EDGE('',*,*,#1794,.T.);
#2603=ORIENTED_EDGE('',*,*,#1909,.T.);
#2604=ORIENTED_EDGE('',*,*,#1913,.T.);
#2605=ORIENTED_EDGE('',*,*,#1898,.F.);
#2606=ORIENTED_EDGE('',*,*,#1800,.F.);
#2607=ORIENTED_EDGE('',*,*,#1804,.T.);
#2608=ORIENTED_EDGE('',*,*,#1914,.T.);
#2609=ORIENTED_EDGE('',*,*,#1889,.F.);
#2610=ORIENTED_EDGE('',*,*,#1812,.F.);
#2611=ORIENTED_EDGE('',*,*,#1843,.F.);
#2612=ORIENTED_EDGE('',*,*,#1914,.F.);
#2613=ORIENTED_EDGE('',*,*,#1811,.F.);
#2614=ORIENTED_EDGE('',*,*,#1913,.F.);
#2615=ORIENTED_EDGE('',*,*,#1792,.T.);
#2616=ORIENTED_EDGE('',*,*,#1894,.F.);
#2617=ORIENTED_EDGE('',*,*,#1915,.T.);
#2618=ORIENTED_EDGE('',*,*,#1900,.T.);
#2619=ORIENTED_EDGE('',*,*,#1916,.T.);
#2620=ORIENTED_EDGE('',*,*,#1906,.T.);
#2621=ORIENTED_EDGE('',*,*,#1917,.F.);
#2622=ORIENTED_EDGE('',*,*,#1788,.T.);
#2623=ORIENTED_EDGE('',*,*,#1802,.F.);
#2624=ORIENTED_EDGE('',*,*,#1918,.T.);
#2625=ORIENTED_EDGE('',*,*,#1896,.T.);
#2626=ORIENTED_EDGE('',*,*,#1919,.T.);
#2627=ORIENTED_EDGE('',*,*,#1904,.F.);
#2628=ORIENTED_EDGE('',*,*,#1920,.T.);
#2629=ORIENTED_EDGE('',*,*,#1789,.F.);
#2630=ORIENTED_EDGE('',*,*,#1895,.T.);
#2631=ORIENTED_EDGE('',*,*,#1917,.T.);
#2632=ORIENTED_EDGE('',*,*,#1905,.F.);
#2633=ORIENTED_EDGE('',*,*,#1919,.F.);
#2634=ORIENTED_EDGE('',*,*,#1915,.F.);
#2635=ORIENTED_EDGE('',*,*,#1893,.F.);
#2636=ORIENTED_EDGE('',*,*,#1837,.F.);
#2637=ORIENTED_EDGE('',*,*,#1901,.F.);
#2638=ORIENTED_EDGE('',*,*,#1796,.F.);
#2639=ORIENTED_EDGE('',*,*,#1897,.F.);
#2640=ORIENTED_EDGE('',*,*,#1918,.F.);
#2641=ORIENTED_EDGE('',*,*,#1801,.F.);
#2642=ORIENTED_EDGE('',*,*,#1798,.F.);
#2643=ORIENTED_EDGE('',*,*,#1803,.F.);
#2644=ORIENTED_EDGE('',*,*,#1920,.F.);
#2645=ORIENTED_EDGE('',*,*,#1903,.F.);
#2646=ORIENTED_EDGE('',*,*,#1916,.F.);
#2647=ORIENTED_EDGE('',*,*,#1902,.F.);
#2648=ORIENTED_EDGE('',*,*,#1841,.F.);
#2649=ORIENTED_EDGE('',*,*,#1907,.F.);
#2650=ORIENTED_EDGE('',*,*,#1921,.F.);
#2651=ORIENTED_EDGE('',*,*,#1922,.T.);
#2652=ORIENTED_EDGE('',*,*,#1923,.T.);
#2653=ORIENTED_EDGE('',*,*,#1922,.F.);
#2654=ORIENTED_EDGE('',*,*,#1924,.F.);
#2655=ORIENTED_EDGE('',*,*,#1925,.T.);
#2656=ORIENTED_EDGE('',*,*,#1926,.T.);
#2657=ORIENTED_EDGE('',*,*,#1927,.T.);
#2658=ORIENTED_EDGE('',*,*,#1928,.T.);
#2659=ORIENTED_EDGE('',*,*,#1929,.F.);
#2660=ORIENTED_EDGE('',*,*,#1930,.T.);
#2661=ORIENTED_EDGE('',*,*,#1931,.T.);
#2662=ORIENTED_EDGE('',*,*,#1932,.T.);
#2663=ORIENTED_EDGE('',*,*,#1933,.T.);
#2664=ORIENTED_EDGE('',*,*,#1931,.F.);
#2665=ORIENTED_EDGE('',*,*,#1934,.T.);
#2666=ORIENTED_EDGE('',*,*,#1924,.T.);
#2667=ORIENTED_EDGE('',*,*,#1935,.T.);
#2668=ORIENTED_EDGE('',*,*,#1936,.T.);
#2669=ORIENTED_EDGE('',*,*,#1923,.F.);
#2670=ORIENTED_EDGE('',*,*,#1937,.T.);
#2671=ORIENTED_EDGE('',*,*,#1929,.T.);
#2672=ORIENTED_EDGE('',*,*,#1938,.T.);
#2673=ORIENTED_EDGE('',*,*,#1939,.T.);
#2674=ORIENTED_EDGE('',*,*,#1926,.F.);
#2675=ORIENTED_EDGE('',*,*,#1921,.T.);
#2676=ORIENTED_EDGE('',*,*,#1940,.F.);
#2677=ORIENTED_EDGE('',*,*,#1927,.F.);
#2678=ORIENTED_EDGE('',*,*,#1941,.F.);
#2679=ORIENTED_EDGE('',*,*,#1941,.T.);
#2680=ORIENTED_EDGE('',*,*,#1939,.F.);
#2681=ORIENTED_EDGE('',*,*,#1942,.F.);
#2682=ORIENTED_EDGE('',*,*,#1943,.F.);
#2683=ORIENTED_EDGE('',*,*,#1928,.F.);
#2684=ORIENTED_EDGE('',*,*,#1940,.T.);
#2685=ORIENTED_EDGE('',*,*,#1944,.F.);
#2686=ORIENTED_EDGE('',*,*,#1938,.F.);
#2687=ORIENTED_EDGE('',*,*,#1933,.F.);
#2688=ORIENTED_EDGE('',*,*,#1945,.F.);
#2689=ORIENTED_EDGE('',*,*,#1942,.T.);
#2690=ORIENTED_EDGE('',*,*,#1944,.T.);
#2691=ORIENTED_EDGE('',*,*,#1943,.T.);
#2692=ORIENTED_EDGE('',*,*,#1946,.F.);
#2693=ORIENTED_EDGE('',*,*,#1935,.F.);
#2694=ORIENTED_EDGE('',*,*,#1946,.T.);
#2695=ORIENTED_EDGE('',*,*,#1945,.T.);
#2696=ORIENTED_EDGE('',*,*,#1932,.F.);
#2697=ORIENTED_EDGE('',*,*,#1936,.F.);
#2698=ORIENTED_EDGE('',*,*,#1925,.F.);
#2699=ORIENTED_EDGE('',*,*,#1934,.F.);
#2700=ORIENTED_EDGE('',*,*,#1930,.F.);
#2701=ORIENTED_EDGE('',*,*,#1937,.F.);
#2702=ORIENTED_EDGE('',*,*,#1947,.F.);
#2703=ORIENTED_EDGE('',*,*,#1948,.T.);
#2704=ORIENTED_EDGE('',*,*,#1949,.F.);
#2705=ORIENTED_EDGE('',*,*,#1948,.F.);
#2706=ORIENTED_EDGE('',*,*,#1950,.T.);
#2707=ORIENTED_EDGE('',*,*,#1951,.T.);
#2708=ORIENTED_EDGE('',*,*,#1952,.T.);
#2709=ORIENTED_EDGE('',*,*,#1953,.T.);
#2710=ORIENTED_EDGE('',*,*,#1954,.T.);
#2711=ORIENTED_EDGE('',*,*,#1955,.T.);
#2712=ORIENTED_EDGE('',*,*,#1956,.T.);
#2713=ORIENTED_EDGE('',*,*,#1957,.T.);
#2714=ORIENTED_EDGE('',*,*,#1958,.T.);
#2715=ORIENTED_EDGE('',*,*,#1959,.T.);
#2716=ORIENTED_EDGE('',*,*,#1960,.T.);
#2717=ORIENTED_EDGE('',*,*,#1961,.T.);
#2718=ORIENTED_EDGE('',*,*,#1962,.T.);
#2719=ORIENTED_EDGE('',*,*,#1963,.T.);
#2720=ORIENTED_EDGE('',*,*,#1964,.T.);
#2721=ORIENTED_EDGE('',*,*,#1965,.T.);
#2722=ORIENTED_EDGE('',*,*,#1966,.T.);
#2723=ORIENTED_EDGE('',*,*,#1967,.T.);
#2724=ORIENTED_EDGE('',*,*,#1968,.T.);
#2725=ORIENTED_EDGE('',*,*,#1969,.T.);
#2726=ORIENTED_EDGE('',*,*,#1970,.F.);
#2727=ORIENTED_EDGE('',*,*,#1971,.T.);
#2728=ORIENTED_EDGE('',*,*,#1972,.T.);
#2729=ORIENTED_EDGE('',*,*,#1973,.T.);
#2730=ORIENTED_EDGE('',*,*,#1974,.T.);
#2731=ORIENTED_EDGE('',*,*,#1975,.F.);
#2732=ORIENTED_EDGE('',*,*,#1976,.T.);
#2733=ORIENTED_EDGE('',*,*,#1977,.T.);
#2734=ORIENTED_EDGE('',*,*,#1978,.T.);
#2735=ORIENTED_EDGE('',*,*,#1979,.F.);
#2736=ORIENTED_EDGE('',*,*,#1980,.T.);
#2737=ORIENTED_EDGE('',*,*,#1977,.F.);
#2738=ORIENTED_EDGE('',*,*,#1981,.T.);
#2739=ORIENTED_EDGE('',*,*,#1970,.T.);
#2740=ORIENTED_EDGE('',*,*,#1982,.T.);
#2741=ORIENTED_EDGE('',*,*,#1983,.T.);
#2742=ORIENTED_EDGE('',*,*,#1947,.T.);
#2743=ORIENTED_EDGE('',*,*,#1984,.T.);
#2744=ORIENTED_EDGE('',*,*,#1975,.T.);
#2745=ORIENTED_EDGE('',*,*,#1985,.T.);
#2746=ORIENTED_EDGE('',*,*,#1986,.T.);
#2747=ORIENTED_EDGE('',*,*,#1972,.F.);
#2748=ORIENTED_EDGE('',*,*,#1949,.T.);
#2749=ORIENTED_EDGE('',*,*,#1951,.F.);
#2750=ORIENTED_EDGE('',*,*,#1987,.F.);
#2751=ORIENTED_EDGE('',*,*,#1973,.F.);
#2752=ORIENTED_EDGE('',*,*,#1988,.F.);
#2753=ORIENTED_EDGE('',*,*,#1989,.F.);
#2754=ORIENTED_EDGE('',*,*,#1953,.F.);
#2755=ORIENTED_EDGE('',*,*,#1990,.F.);
#2756=ORIENTED_EDGE('',*,*,#1988,.T.);
#2757=ORIENTED_EDGE('',*,*,#1986,.F.);
#2758=ORIENTED_EDGE('',*,*,#1991,.F.);
#2759=ORIENTED_EDGE('',*,*,#1962,.F.);
#2760=ORIENTED_EDGE('',*,*,#1992,.F.);
#2761=ORIENTED_EDGE('',*,*,#1959,.F.);
#2762=ORIENTED_EDGE('',*,*,#1993,.F.);
#2763=ORIENTED_EDGE('',*,*,#1957,.F.);
#2764=ORIENTED_EDGE('',*,*,#1994,.F.);
#2765=ORIENTED_EDGE('',*,*,#1955,.F.);
#2766=ORIENTED_EDGE('',*,*,#1995,.F.);
#2767=ORIENTED_EDGE('',*,*,#1950,.F.);
#2768=ORIENTED_EDGE('',*,*,#1989,.T.);
#2769=ORIENTED_EDGE('',*,*,#1996,.F.);
#2770=ORIENTED_EDGE('',*,*,#1974,.F.);
#2771=ORIENTED_EDGE('',*,*,#1987,.T.);
#2772=ORIENTED_EDGE('',*,*,#1997,.F.);
#2773=ORIENTED_EDGE('',*,*,#1998,.F.);
#2774=ORIENTED_EDGE('',*,*,#1965,.F.);
#2775=ORIENTED_EDGE('',*,*,#1999,.F.);
#2776=ORIENTED_EDGE('',*,*,#1967,.F.);
#2777=ORIENTED_EDGE('',*,*,#2000,.F.);
#2778=ORIENTED_EDGE('',*,*,#1969,.F.);
#2779=ORIENTED_EDGE('',*,*,#2001,.F.);
#2780=ORIENTED_EDGE('',*,*,#1963,.F.);
#2781=ORIENTED_EDGE('',*,*,#1991,.T.);
#2782=ORIENTED_EDGE('',*,*,#1985,.F.);
#2783=ORIENTED_EDGE('',*,*,#1980,.F.);
#2784=ORIENTED_EDGE('',*,*,#1952,.F.);
#2785=ORIENTED_EDGE('',*,*,#1995,.T.);
#2786=ORIENTED_EDGE('',*,*,#1954,.F.);
#2787=ORIENTED_EDGE('',*,*,#1994,.T.);
#2788=ORIENTED_EDGE('',*,*,#1956,.F.);
#2789=ORIENTED_EDGE('',*,*,#1993,.T.);
#2790=ORIENTED_EDGE('',*,*,#1958,.F.);
#2791=ORIENTED_EDGE('',*,*,#1992,.T.);
#2792=ORIENTED_EDGE('',*,*,#1961,.F.);
#2793=ORIENTED_EDGE('',*,*,#2002,.F.);
#2794=ORIENTED_EDGE('',*,*,#1982,.F.);
#2795=ORIENTED_EDGE('',*,*,#1996,.T.);
#2796=ORIENTED_EDGE('',*,*,#1990,.T.);
#2797=ORIENTED_EDGE('',*,*,#2003,.F.);
#2798=ORIENTED_EDGE('',*,*,#1978,.F.);
#2799=ORIENTED_EDGE('',*,*,#1983,.F.);
#2800=ORIENTED_EDGE('',*,*,#2002,.T.);
#2801=ORIENTED_EDGE('',*,*,#1960,.F.);
#2802=ORIENTED_EDGE('',*,*,#2001,.T.);
#2803=ORIENTED_EDGE('',*,*,#1968,.F.);
#2804=ORIENTED_EDGE('',*,*,#2000,.T.);
#2805=ORIENTED_EDGE('',*,*,#1966,.F.);
#2806=ORIENTED_EDGE('',*,*,#1999,.T.);
#2807=ORIENTED_EDGE('',*,*,#1964,.F.);
#2808=ORIENTED_EDGE('',*,*,#1998,.T.);
#2809=ORIENTED_EDGE('',*,*,#1979,.T.);
#2810=ORIENTED_EDGE('',*,*,#2003,.T.);
#2811=ORIENTED_EDGE('',*,*,#1997,.T.);
#2812=ORIENTED_EDGE('',*,*,#1971,.F.);
#2813=ORIENTED_EDGE('',*,*,#1981,.F.);
#2814=ORIENTED_EDGE('',*,*,#1976,.F.);
#2815=ORIENTED_EDGE('',*,*,#1984,.F.);
#2816=ORIENTED_EDGE('',*,*,#2004,.F.);
#2817=ORIENTED_EDGE('',*,*,#2005,.T.);
#2818=ORIENTED_EDGE('',*,*,#2006,.T.);
#2819=ORIENTED_EDGE('',*,*,#2005,.F.);
#2820=ORIENTED_EDGE('',*,*,#2007,.T.);
#2821=ORIENTED_EDGE('',*,*,#2008,.T.);
#2822=ORIENTED_EDGE('',*,*,#2009,.T.);
#2823=ORIENTED_EDGE('',*,*,#2010,.T.);
#2824=ORIENTED_EDGE('',*,*,#2011,.F.);
#2825=ORIENTED_EDGE('',*,*,#2012,.F.);
#2826=ORIENTED_EDGE('',*,*,#2013,.F.);
#2827=ORIENTED_EDGE('',*,*,#2014,.F.);
#2828=ORIENTED_EDGE('',*,*,#2015,.F.);
#2829=ORIENTED_EDGE('',*,*,#2016,.F.);
#2830=ORIENTED_EDGE('',*,*,#2010,.F.);
#2831=ORIENTED_EDGE('',*,*,#2017,.T.);
#2832=ORIENTED_EDGE('',*,*,#2018,.T.);
#2833=ORIENTED_EDGE('',*,*,#2019,.T.);
#2834=ORIENTED_EDGE('',*,*,#2020,.F.);
#2835=ORIENTED_EDGE('',*,*,#2021,.T.);
#2836=ORIENTED_EDGE('',*,*,#2007,.F.);
#2837=ORIENTED_EDGE('',*,*,#2022,.T.);
#2838=ORIENTED_EDGE('',*,*,#2023,.T.);
#2839=ORIENTED_EDGE('',*,*,#2017,.F.);
#2840=ORIENTED_EDGE('',*,*,#2019,.F.);
#2841=ORIENTED_EDGE('',*,*,#2024,.T.);
#2842=ORIENTED_EDGE('',*,*,#2025,.F.);
#2843=ORIENTED_EDGE('',*,*,#2026,.F.);
#2844=ORIENTED_EDGE('',*,*,#2027,.T.);
#2845=ORIENTED_EDGE('',*,*,#2028,.T.);
#2846=ORIENTED_EDGE('',*,*,#2029,.T.);
#2847=ORIENTED_EDGE('',*,*,#2030,.T.);
#2848=ORIENTED_EDGE('',*,*,#2031,.T.);
#2849=ORIENTED_EDGE('',*,*,#2032,.F.);
#2850=ORIENTED_EDGE('',*,*,#2033,.T.);
#2851=ORIENTED_EDGE('',*,*,#2034,.T.);
#2852=ORIENTED_EDGE('',*,*,#2035,.T.);
#2853=ORIENTED_EDGE('',*,*,#2036,.T.);
#2854=ORIENTED_EDGE('',*,*,#2037,.T.);
#2855=ORIENTED_EDGE('',*,*,#2009,.F.);
#2856=ORIENTED_EDGE('',*,*,#2038,.T.);
#2857=ORIENTED_EDGE('',*,*,#2039,.T.);
#2858=ORIENTED_EDGE('',*,*,#2028,.F.);
#2859=ORIENTED_EDGE('',*,*,#2040,.T.);
#2860=ORIENTED_EDGE('',*,*,#2032,.T.);
#2861=ORIENTED_EDGE('',*,*,#2041,.T.);
#2862=ORIENTED_EDGE('',*,*,#2020,.T.);
#2863=ORIENTED_EDGE('',*,*,#2025,.T.);
#2864=ORIENTED_EDGE('',*,*,#2042,.T.);
#2865=ORIENTED_EDGE('',*,*,#2006,.F.);
#2866=ORIENTED_EDGE('',*,*,#2043,.T.);
#2867=ORIENTED_EDGE('',*,*,#2026,.T.);
#2868=ORIENTED_EDGE('',*,*,#2044,.T.);
#2869=ORIENTED_EDGE('',*,*,#2022,.F.);
#2870=ORIENTED_EDGE('',*,*,#2039,.F.);
#2871=ORIENTED_EDGE('',*,*,#2045,.T.);
#2872=ORIENTED_EDGE('',*,*,#2034,.F.);
#2873=ORIENTED_EDGE('',*,*,#2004,.T.);
#2874=ORIENTED_EDGE('',*,*,#2046,.T.);
#2875=ORIENTED_EDGE('',*,*,#2047,.T.);
#2876=ORIENTED_EDGE('',*,*,#2048,.T.);
#2877=ORIENTED_EDGE('',*,*,#2049,.F.);
#2878=ORIENTED_EDGE('',*,*,#2050,.F.);
#2879=ORIENTED_EDGE('',*,*,#2051,.T.);
#2880=ORIENTED_EDGE('',*,*,#2052,.T.);
#2881=ORIENTED_EDGE('',*,*,#2050,.T.);
#2882=ORIENTED_EDGE('',*,*,#2053,.F.);
#2883=ORIENTED_EDGE('',*,*,#2054,.F.);
#2884=ORIENTED_EDGE('',*,*,#2055,.T.);
#2885=ORIENTED_EDGE('',*,*,#2056,.T.);
#2886=ORIENTED_EDGE('',*,*,#2054,.T.);
#2887=ORIENTED_EDGE('',*,*,#2057,.F.);
#2888=ORIENTED_EDGE('',*,*,#2058,.F.);
#2889=ORIENTED_EDGE('',*,*,#2059,.T.);
#2890=ORIENTED_EDGE('',*,*,#2060,.T.);
#2891=ORIENTED_EDGE('',*,*,#2058,.T.);
#2892=ORIENTED_EDGE('',*,*,#2061,.F.);
#2893=ORIENTED_EDGE('',*,*,#2062,.F.);
#2894=ORIENTED_EDGE('',*,*,#2063,.T.);
#2895=ORIENTED_EDGE('',*,*,#2064,.T.);
#2896=ORIENTED_EDGE('',*,*,#2062,.T.);
#2897=ORIENTED_EDGE('',*,*,#2065,.F.);
#2898=ORIENTED_EDGE('',*,*,#2066,.F.);
#2899=ORIENTED_EDGE('',*,*,#2067,.T.);
#2900=ORIENTED_EDGE('',*,*,#2068,.T.);
#2901=ORIENTED_EDGE('',*,*,#2066,.T.);
#2902=ORIENTED_EDGE('',*,*,#2069,.F.);
#2903=ORIENTED_EDGE('',*,*,#2048,.F.);
#2904=ORIENTED_EDGE('',*,*,#2052,.F.);
#2905=ORIENTED_EDGE('',*,*,#2016,.T.);
#2906=ORIENTED_EDGE('',*,*,#2046,.F.);
#2907=ORIENTED_EDGE('',*,*,#2047,.F.);
#2908=ORIENTED_EDGE('',*,*,#2015,.T.);
#2909=ORIENTED_EDGE('',*,*,#2067,.F.);
#2910=ORIENTED_EDGE('',*,*,#2068,.F.);
#2911=ORIENTED_EDGE('',*,*,#2014,.T.);
#2912=ORIENTED_EDGE('',*,*,#2063,.F.);
#2913=ORIENTED_EDGE('',*,*,#2064,.F.);
#2914=ORIENTED_EDGE('',*,*,#2013,.T.);
#2915=ORIENTED_EDGE('',*,*,#2059,.F.);
#2916=ORIENTED_EDGE('',*,*,#2060,.F.);
#2917=ORIENTED_EDGE('',*,*,#2012,.T.);
#2918=ORIENTED_EDGE('',*,*,#2055,.F.);
#2919=ORIENTED_EDGE('',*,*,#2056,.F.);
#2920=ORIENTED_EDGE('',*,*,#2011,.T.);
#2921=ORIENTED_EDGE('',*,*,#2051,.F.);
#2922=ORIENTED_EDGE('',*,*,#2057,.T.);
#2923=ORIENTED_EDGE('',*,*,#2053,.T.);
#2924=ORIENTED_EDGE('',*,*,#2049,.T.);
#2925=ORIENTED_EDGE('',*,*,#2069,.T.);
#2926=ORIENTED_EDGE('',*,*,#2065,.T.);
#2927=ORIENTED_EDGE('',*,*,#2061,.T.);
#2928=ORIENTED_EDGE('',*,*,#2044,.F.);
#2929=ORIENTED_EDGE('',*,*,#2031,.F.);
#2930=ORIENTED_EDGE('',*,*,#2070,.F.);
#2931=ORIENTED_EDGE('',*,*,#2023,.F.);
#2932=ORIENTED_EDGE('',*,*,#2070,.T.);
#2933=ORIENTED_EDGE('',*,*,#2030,.F.);
#2934=ORIENTED_EDGE('',*,*,#2071,.F.);
#2935=ORIENTED_EDGE('',*,*,#2018,.F.);
#2936=ORIENTED_EDGE('',*,*,#2042,.F.);
#2937=ORIENTED_EDGE('',*,*,#2024,.F.);
#2938=ORIENTED_EDGE('',*,*,#2071,.T.);
#2939=ORIENTED_EDGE('',*,*,#2029,.F.);
#2940=ORIENTED_EDGE('',*,*,#2045,.F.);
#2941=ORIENTED_EDGE('',*,*,#2038,.F.);
#2942=ORIENTED_EDGE('',*,*,#2072,.F.);
#2943=ORIENTED_EDGE('',*,*,#2035,.F.);
#2944=ORIENTED_EDGE('',*,*,#2072,.T.);
#2945=ORIENTED_EDGE('',*,*,#2008,.F.);
#2946=ORIENTED_EDGE('',*,*,#2073,.F.);
#2947=ORIENTED_EDGE('',*,*,#2036,.F.);
#2948=ORIENTED_EDGE('',*,*,#2041,.F.);
#2949=ORIENTED_EDGE('',*,*,#2037,.F.);
#2950=ORIENTED_EDGE('',*,*,#2073,.T.);
#2951=ORIENTED_EDGE('',*,*,#2021,.F.);
#2952=ORIENTED_EDGE('',*,*,#2033,.F.);
#2953=ORIENTED_EDGE('',*,*,#2040,.F.);
#2954=ORIENTED_EDGE('',*,*,#2027,.F.);
#2955=ORIENTED_EDGE('',*,*,#2043,.F.);
#2956=ORIENTED_EDGE('',*,*,#2074,.F.);
#2957=ORIENTED_EDGE('',*,*,#2075,.T.);
#2958=ORIENTED_EDGE('',*,*,#2076,.F.);
#2959=ORIENTED_EDGE('',*,*,#2075,.F.);
#2960=ORIENTED_EDGE('',*,*,#2077,.F.);
#2961=ORIENTED_EDGE('',*,*,#2078,.T.);
#2962=ORIENTED_EDGE('',*,*,#2079,.T.);
#2963=ORIENTED_EDGE('',*,*,#2080,.F.);
#2964=ORIENTED_EDGE('',*,*,#2081,.F.);
#2965=ORIENTED_EDGE('',*,*,#2082,.T.);
#2966=ORIENTED_EDGE('',*,*,#2083,.T.);
#2967=ORIENTED_EDGE('',*,*,#2084,.T.);
#2968=ORIENTED_EDGE('',*,*,#2085,.F.);
#2969=ORIENTED_EDGE('',*,*,#2086,.T.);
#2970=ORIENTED_EDGE('',*,*,#2087,.T.);
#2971=ORIENTED_EDGE('',*,*,#2088,.T.);
#2972=ORIENTED_EDGE('',*,*,#2077,.T.);
#2973=ORIENTED_EDGE('',*,*,#2089,.F.);
#2974=ORIENTED_EDGE('',*,*,#2081,.T.);
#2975=ORIENTED_EDGE('',*,*,#2090,.T.);
#2976=ORIENTED_EDGE('',*,*,#2074,.T.);
#2977=ORIENTED_EDGE('',*,*,#2091,.T.);
#2978=ORIENTED_EDGE('',*,*,#2092,.T.);
#2979=ORIENTED_EDGE('',*,*,#2093,.T.);
#2980=ORIENTED_EDGE('',*,*,#2083,.F.);
#2981=ORIENTED_EDGE('',*,*,#2094,.F.);
#2982=ORIENTED_EDGE('',*,*,#2079,.F.);
#2983=ORIENTED_EDGE('',*,*,#2095,.T.);
#2984=ORIENTED_EDGE('',*,*,#2096,.F.);
#2985=ORIENTED_EDGE('',*,*,#2076,.T.);
#2986=ORIENTED_EDGE('',*,*,#2089,.T.);
#2987=ORIENTED_EDGE('',*,*,#2080,.T.);
#2988=ORIENTED_EDGE('',*,*,#2094,.T.);
#2989=ORIENTED_EDGE('',*,*,#2082,.F.);
#2990=ORIENTED_EDGE('',*,*,#2087,.F.);
#2991=ORIENTED_EDGE('',*,*,#2097,.T.);
#2992=ORIENTED_EDGE('',*,*,#2096,.T.);
#2993=ORIENTED_EDGE('',*,*,#2098,.F.);
#2994=ORIENTED_EDGE('',*,*,#2092,.F.);
#2995=ORIENTED_EDGE('',*,*,#2099,.T.);
#2996=ORIENTED_EDGE('',*,*,#2085,.T.);
#2997=ORIENTED_EDGE('',*,*,#2100,.T.);
#2998=ORIENTED_EDGE('',*,*,#2078,.F.);
#2999=ORIENTED_EDGE('',*,*,#2088,.F.);
#3000=ORIENTED_EDGE('',*,*,#2098,.T.);
#3001=ORIENTED_EDGE('',*,*,#2095,.F.);
#3002=ORIENTED_EDGE('',*,*,#2084,.F.);
#3003=ORIENTED_EDGE('',*,*,#2093,.F.);
#3004=ORIENTED_EDGE('',*,*,#2100,.F.);
#3005=ORIENTED_EDGE('',*,*,#2090,.F.);
#3006=ORIENTED_EDGE('',*,*,#2097,.F.);
#3007=ORIENTED_EDGE('',*,*,#2086,.F.);
#3008=ORIENTED_EDGE('',*,*,#2099,.F.);
#3009=ORIENTED_EDGE('',*,*,#2091,.F.);
#3010=ORIENTED_EDGE('',*,*,#2101,.F.);
#3011=ORIENTED_EDGE('',*,*,#2102,.T.);
#3012=ORIENTED_EDGE('',*,*,#2103,.T.);
#3013=ORIENTED_EDGE('',*,*,#2102,.F.);
#3014=ORIENTED_EDGE('',*,*,#2104,.T.);
#3015=ORIENTED_EDGE('',*,*,#2105,.T.);
#3016=ORIENTED_EDGE('',*,*,#2106,.F.);
#3017=ORIENTED_EDGE('',*,*,#2105,.F.);
#3018=ORIENTED_EDGE('',*,*,#2107,.T.);
#3019=ORIENTED_EDGE('',*,*,#2108,.T.);
#3020=ORIENTED_EDGE('',*,*,#2109,.F.);
#3021=ORIENTED_EDGE('',*,*,#2108,.F.);
#3022=ORIENTED_EDGE('',*,*,#2106,.T.);
#3023=ORIENTED_EDGE('',*,*,#2104,.F.);
#3024=ORIENTED_EDGE('',*,*,#2109,.T.);
#3025=ORIENTED_EDGE('',*,*,#2103,.F.);
#3026=ORIENTED_EDGE('',*,*,#2101,.T.);
#3027=ORIENTED_EDGE('',*,*,#2107,.F.);
#3028=CYLINDRICAL_SURFACE('',#3356,2.);
#3029=CYLINDRICAL_SURFACE('',#3359,2.);
#3030=CYLINDRICAL_SURFACE('',#3362,2.);
#3031=CYLINDRICAL_SURFACE('',#3365,2.);
#3032=CYLINDRICAL_SURFACE('',#3413,1.);
#3033=CYLINDRICAL_SURFACE('',#3414,1.);
#3034=CYLINDRICAL_SURFACE('',#3415,1.);
#3035=CYLINDRICAL_SURFACE('',#3416,1.);
#3036=CYLINDRICAL_SURFACE('',#3417,1.);
#3037=CYLINDRICAL_SURFACE('',#3418,1.);
#3038=CYLINDRICAL_SURFACE('',#3419,1.);
#3039=CYLINDRICAL_SURFACE('',#3420,1.);
#3040=CYLINDRICAL_SURFACE('',#3421,1.);
#3041=CYLINDRICAL_SURFACE('',#3433,3.5);
#3042=CYLINDRICAL_SURFACE('',#3434,3.5);
#3043=CYLINDRICAL_SURFACE('',#3435,3.5);
#3044=CYLINDRICAL_SURFACE('',#3436,3.5);
#3045=CYLINDRICAL_SURFACE('',#3438,2.);
#3046=CYLINDRICAL_SURFACE('',#3441,2.);
#3047=CYLINDRICAL_SURFACE('',#3444,2.);
#3048=CYLINDRICAL_SURFACE('',#3493,1.);
#3049=CYLINDRICAL_SURFACE('',#3494,1.);
#3050=CYLINDRICAL_SURFACE('',#3495,1.);
#3051=CYLINDRICAL_SURFACE('',#3496,1.);
#3052=CYLINDRICAL_SURFACE('',#3497,1.);
#3053=CYLINDRICAL_SURFACE('',#3498,1.);
#3054=CYLINDRICAL_SURFACE('',#3499,1.);
#3055=CYLINDRICAL_SURFACE('',#3500,1.);
#3056=CYLINDRICAL_SURFACE('',#3501,1.);
#3057=CYLINDRICAL_SURFACE('',#3515,3.5);
#3058=CYLINDRICAL_SURFACE('',#3516,3.5);
#3059=CYLINDRICAL_SURFACE('',#3517,3.5);
#3060=CYLINDRICAL_SURFACE('',#3518,3.5);
#3061=CYLINDRICAL_SURFACE('',#3520,2.);
#3062=CYLINDRICAL_SURFACE('',#3539,3.5);
#3063=CYLINDRICAL_SURFACE('',#3541,2.);
#3064=CYLINDRICAL_SURFACE('',#3544,0.999999999998776);
#3065=CYLINDRICAL_SURFACE('',#3545,0.999999999998766);
#3066=CYLINDRICAL_SURFACE('',#3548,0.999999999998766);
#3067=CYLINDRICAL_SURFACE('',#3551,0.999999999998766);
#3068=CYLINDRICAL_SURFACE('',#3554,0.999999999998766);
#3069=CYLINDRICAL_SURFACE('',#3557,0.999999999998766);
#3070=CYLINDRICAL_SURFACE('',#3560,1.);
#3071=CYLINDRICAL_SURFACE('',#3561,1.00000000000001);
#3072=CYLINDRICAL_SURFACE('',#3562,0.999999999999161);
#3073=CYLINDRICAL_SURFACE('',#3583,1.);
#3074=CYLINDRICAL_SURFACE('',#3584,3.5);
#3075=CYLINDRICAL_SURFACE('',#3586,2.);
#3076=CYLINDRICAL_SURFACE('',#3589,1.);
#3077=CYLINDRICAL_SURFACE('',#3629,3.);
#3078=CYLINDRICAL_SURFACE('',#3632,3.);
#3079=CYLINDRICAL_SURFACE('',#3633,3.);
#3080=CYLINDRICAL_SURFACE('',#3636,3.);
#3081=CYLINDRICAL_SURFACE('',#3637,3.5);
#3082=CYLINDRICAL_SURFACE('',#3639,2.);
#3083=CYLINDRICAL_SURFACE('',#3642,10.);
#3084=CYLINDRICAL_SURFACE('',#3645,5.);
#3085=CYLINDRICAL_SURFACE('',#3659,10.);
#3086=CYLINDRICAL_SURFACE('',#3660,10.);
#3087=CYLINDRICAL_SURFACE('',#3661,3.5);
#3088=CYLINDRICAL_SURFACE('',#3663,3.);
#3089=CYLINDRICAL_SURFACE('',#3666,3.);
#3090=CYLINDRICAL_SURFACE('',#3669,2.);
#3091=ADVANCED_FACE('',(#242),#3028,.F.);
#3092=ADVANCED_FACE('',(#243),#3029,.F.);
#3093=ADVANCED_FACE('',(#244),#3030,.F.);
#3094=ADVANCED_FACE('',(#245),#3031,.F.);
#3095=ADVANCED_FACE('',(#246),#137,.F.);
#3096=ADVANCED_FACE('',(#247),#138,.F.);
#3097=ADVANCED_FACE('',(#248,#113,#114),#139,.F.);
#3098=ADVANCED_FACE('',(#249,#115,#116),#140,.T.);
#3099=ADVANCED_FACE('',(#250),#141,.F.);
#3100=ADVANCED_FACE('',(#251),#142,.F.);
#3101=ADVANCED_FACE('',(#252),#143,.F.);
#3102=ADVANCED_FACE('',(#253),#144,.F.);
#3103=ADVANCED_FACE('',(#254),#145,.F.);
#3104=ADVANCED_FACE('',(#255),#146,.F.);
#3105=ADVANCED_FACE('',(#256),#147,.F.);
#3106=ADVANCED_FACE('',(#257),#148,.F.);
#3107=ADVANCED_FACE('',(#258),#149,.F.);
#3108=ADVANCED_FACE('',(#259),#150,.F.);
#3109=ADVANCED_FACE('',(#260),#151,.F.);
#3110=ADVANCED_FACE('',(#261),#152,.F.);
#3111=ADVANCED_FACE('',(#262),#153,.F.);
#3112=ADVANCED_FACE('',(#263),#154,.F.);
#3113=ADVANCED_FACE('',(#264),#155,.F.);
#3114=ADVANCED_FACE('',(#265),#156,.F.);
#3115=ADVANCED_FACE('',(#266),#157,.F.);
#3116=ADVANCED_FACE('',(#267),#158,.F.);
#3117=ADVANCED_FACE('',(#268),#159,.F.);
#3118=ADVANCED_FACE('',(#269),#3032,.F.);
#3119=ADVANCED_FACE('',(#270),#3033,.F.);
#3120=ADVANCED_FACE('',(#271),#3034,.F.);
#3121=ADVANCED_FACE('',(#272),#3035,.F.);
#3122=ADVANCED_FACE('',(#273),#3036,.F.);
#3123=ADVANCED_FACE('',(#274),#3037,.F.);
#3124=ADVANCED_FACE('',(#275),#3038,.F.);
#3125=ADVANCED_FACE('',(#276),#3039,.F.);
#3126=ADVANCED_FACE('',(#277),#3040,.F.);
#3127=ADVANCED_FACE('',(#278),#160,.F.);
#3128=ADVANCED_FACE('',(#279),#161,.F.);
#3129=ADVANCED_FACE('',(#280,#117),#162,.T.);
#3130=ADVANCED_FACE('',(#281,#118),#163,.F.);
#3131=ADVANCED_FACE('',(#282,#119),#164,.F.);
#3132=ADVANCED_FACE('',(#283,#120),#165,.T.);
#3133=ADVANCED_FACE('',(#284),#166,.T.);
#3134=ADVANCED_FACE('',(#285),#3041,.T.);
#3135=ADVANCED_FACE('',(#286),#3042,.T.);
#3136=ADVANCED_FACE('',(#287),#3043,.T.);
#3137=ADVANCED_FACE('',(#288),#3044,.T.);
#3138=ADVANCED_FACE('',(#289),#3045,.F.);
#3139=ADVANCED_FACE('',(#290),#3046,.F.);
#3140=ADVANCED_FACE('',(#291),#3047,.F.);
#3141=ADVANCED_FACE('',(#292,#121),#167,.F.);
#3142=ADVANCED_FACE('',(#293),#168,.F.);
#3143=ADVANCED_FACE('',(#294),#169,.F.);
#3144=ADVANCED_FACE('',(#295),#170,.F.);
#3145=ADVANCED_FACE('',(#296,#122),#171,.T.);
#3146=ADVANCED_FACE('',(#297),#172,.F.);
#3147=ADVANCED_FACE('',(#298),#173,.T.);
#3148=ADVANCED_FACE('',(#299),#174,.F.);
#3149=ADVANCED_FACE('',(#300),#175,.F.);
#3150=ADVANCED_FACE('',(#301),#176,.F.);
#3151=ADVANCED_FACE('',(#302),#177,.F.);
#3152=ADVANCED_FACE('',(#303),#178,.F.);
#3153=ADVANCED_FACE('',(#304),#179,.F.);
#3154=ADVANCED_FACE('',(#305),#180,.F.);
#3155=ADVANCED_FACE('',(#306),#181,.F.);
#3156=ADVANCED_FACE('',(#307),#182,.F.);
#3157=ADVANCED_FACE('',(#308),#183,.F.);
#3158=ADVANCED_FACE('',(#309),#184,.F.);
#3159=ADVANCED_FACE('',(#310),#185,.F.);
#3160=ADVANCED_FACE('',(#311),#186,.F.);
#3161=ADVANCED_FACE('',(#312),#187,.F.);
#3162=ADVANCED_FACE('',(#313),#188,.F.);
#3163=ADVANCED_FACE('',(#314),#189,.F.);
#3164=ADVANCED_FACE('',(#315),#190,.F.);
#3165=ADVANCED_FACE('',(#316),#3048,.F.);
#3166=ADVANCED_FACE('',(#317),#3049,.F.);
#3167=ADVANCED_FACE('',(#318),#3050,.F.);
#3168=ADVANCED_FACE('',(#319),#3051,.F.);
#3169=ADVANCED_FACE('',(#320),#3052,.F.);
#3170=ADVANCED_FACE('',(#321),#3053,.F.);
#3171=ADVANCED_FACE('',(#322),#3054,.F.);
#3172=ADVANCED_FACE('',(#323),#3055,.F.);
#3173=ADVANCED_FACE('',(#324),#3056,.F.);
#3174=ADVANCED_FACE('',(#325),#191,.T.);
#3175=ADVANCED_FACE('',(#326),#192,.T.);
#3176=ADVANCED_FACE('',(#327,#123),#193,.F.);
#3177=ADVANCED_FACE('',(#328),#194,.T.);
#3178=ADVANCED_FACE('',(#329),#195,.T.);
#3179=ADVANCED_FACE('',(#330,#124),#196,.F.);
#3180=ADVANCED_FACE('',(#331,#125),#197,.F.);
#3181=ADVANCED_FACE('',(#332,#126),#198,.T.);
#3182=ADVANCED_FACE('',(#333),#199,.T.);
#3183=ADVANCED_FACE('',(#334),#3057,.T.);
#3184=ADVANCED_FACE('',(#335),#3058,.T.);
#3185=ADVANCED_FACE('',(#336),#3059,.T.);
#3186=ADVANCED_FACE('',(#337),#3060,.T.);
#3187=ADVANCED_FACE('',(#338),#3061,.F.);
#3188=ADVANCED_FACE('',(#339),#200,.F.);
#3189=ADVANCED_FACE('',(#340),#201,.T.);
#3190=ADVANCED_FACE('',(#341,#127),#202,.T.);
#3191=ADVANCED_FACE('',(#342,#128),#203,.F.);
#3192=ADVANCED_FACE('',(#343),#73,.T.);
#3193=ADVANCED_FACE('',(#344),#204,.T.);
#3194=ADVANCED_FACE('',(#345),#74,.T.);
#3195=ADVANCED_FACE('',(#346),#75,.T.);
#3196=ADVANCED_FACE('',(#347),#205,.F.);
#3197=ADVANCED_FACE('',(#348),#76,.T.);
#3198=ADVANCED_FACE('',(#349),#3062,.T.);
#3199=ADVANCED_FACE('',(#350),#3063,.F.);
#3200=ADVANCED_FACE('',(#351),#3064,.F.);
#3201=ADVANCED_FACE('',(#352),#3065,.F.);
#3202=ADVANCED_FACE('',(#353),#3066,.F.);
#3203=ADVANCED_FACE('',(#354),#3067,.F.);
#3204=ADVANCED_FACE('',(#355),#3068,.F.);
#3205=ADVANCED_FACE('',(#356),#3069,.F.);
#3206=ADVANCED_FACE('',(#357),#3070,.F.);
#3207=ADVANCED_FACE('',(#358),#3071,.F.);
#3208=ADVANCED_FACE('',(#359),#3072,.F.);
#3209=ADVANCED_FACE('',(#360),#206,.F.);
#3210=ADVANCED_FACE('',(#361),#207,.T.);
#3211=ADVANCED_FACE('',(#362,#129),#208,.T.);
#3212=ADVANCED_FACE('',(#363,#130),#209,.F.);
#3213=ADVANCED_FACE('',(#364),#77,.T.);
#3214=ADVANCED_FACE('',(#365),#210,.T.);
#3215=ADVANCED_FACE('',(#366),#78,.T.);
#3216=ADVANCED_FACE('',(#367),#79,.T.);
#3217=ADVANCED_FACE('',(#368),#211,.F.);
#3218=ADVANCED_FACE('',(#369),#80,.T.);
#3219=ADVANCED_FACE('',(#370),#3073,.F.);
#3220=ADVANCED_FACE('',(#371),#3074,.T.);
#3221=ADVANCED_FACE('',(#372),#3075,.F.);
#3222=ADVANCED_FACE('',(#373),#3076,.T.);
#3223=ADVANCED_FACE('',(#374),#212,.F.);
#3224=ADVANCED_FACE('',(#375),#213,.F.);
#3225=ADVANCED_FACE('',(#376),#214,.F.);
#3226=ADVANCED_FACE('',(#377),#215,.T.);
#3227=ADVANCED_FACE('',(#378),#216,.F.);
#3228=ADVANCED_FACE('',(#379),#217,.F.);
#3229=ADVANCED_FACE('',(#380,#131),#218,.T.);
#3230=ADVANCED_FACE('',(#381,#132),#219,.F.);
#3231=ADVANCED_FACE('',(#382),#220,.T.);
#3232=ADVANCED_FACE('',(#383),#221,.T.);
#3233=ADVANCED_FACE('',(#384),#222,.T.);
#3234=ADVANCED_FACE('',(#385),#223,.T.);
#3235=ADVANCED_FACE('',(#386),#224,.T.);
#3236=ADVANCED_FACE('',(#387),#225,.T.);
#3237=ADVANCED_FACE('',(#388),#226,.F.);
#3238=ADVANCED_FACE('',(#389),#227,.F.);
#3239=ADVANCED_FACE('',(#390),#228,.F.);
#3240=ADVANCED_FACE('',(#391),#229,.F.);
#3241=ADVANCED_FACE('',(#392),#230,.F.);
#3242=ADVANCED_FACE('',(#393),#231,.F.);
#3243=ADVANCED_FACE('',(#394),#232,.T.);
#3244=ADVANCED_FACE('',(#395),#3077,.T.);
#3245=ADVANCED_FACE('',(#396),#47,.T.);
#3246=ADVANCED_FACE('',(#397),#3078,.T.);
#3247=ADVANCED_FACE('',(#398),#3079,.T.);
#3248=ADVANCED_FACE('',(#399),#48,.T.);
#3249=ADVANCED_FACE('',(#400),#3080,.T.);
#3250=ADVANCED_FACE('',(#401),#3081,.T.);
#3251=ADVANCED_FACE('',(#402),#3082,.F.);
#3252=ADVANCED_FACE('',(#403),#3083,.F.);
#3253=ADVANCED_FACE('',(#404),#3084,.F.);
#3254=ADVANCED_FACE('',(#405,#133),#233,.T.);
#3255=ADVANCED_FACE('',(#406,#134),#234,.F.);
#3256=ADVANCED_FACE('',(#407),#235,.T.);
#3257=ADVANCED_FACE('',(#408),#236,.F.);
#3258=ADVANCED_FACE('',(#409),#237,.T.);
#3259=ADVANCED_FACE('',(#410),#3085,.T.);
#3260=ADVANCED_FACE('',(#411),#3086,.T.);
#3261=ADVANCED_FACE('',(#412),#3087,.T.);
#3262=ADVANCED_FACE('',(#413),#3088,.T.);
#3263=ADVANCED_FACE('',(#414),#3089,.T.);
#3264=ADVANCED_FACE('',(#415),#3090,.T.);
#3265=ADVANCED_FACE('',(#416),#238,.T.);
#3266=ADVANCED_FACE('',(#417,#135),#239,.F.);
#3267=ADVANCED_FACE('',(#418),#240,.T.);
#3268=ADVANCED_FACE('',(#419,#136),#241,.F.);
#3269=CLOSED_SHELL('',(#3091,#3092,#3093,#3094,#3095,#3096,#3097,#3098,
#3099,#3100,#3101,#3102,#3103,#3104,#3105,#3106,#3107,#3108,#3109,#3110,
#3111,#3112,#3113,#3114,#3115,#3116,#3117,#3118,#3119,#3120,#3121,#3122,
#3123,#3124,#3125,#3126,#3127,#3128,#3129,#3130,#3131,#3132,#3133,#3134,
#3135,#3136,#3137));
#3270=CLOSED_SHELL('',(#3138,#3139,#3140,#3141,#3142,#3143,#3144,#3145,
#3146,#3147,#3148,#3149,#3150,#3151,#3152,#3153,#3154,#3155,#3156,#3157,
#3158,#3159,#3160,#3161,#3162,#3163,#3164,#3165,#3166,#3167,#3168,#3169,
#3170,#3171,#3172,#3173,#3174,#3175,#3176,#3177,#3178,#3179,#3180,#3181,
#3182,#3183,#3184,#3185,#3186));
#3271=CLOSED_SHELL('',(#3187,#3188,#3189,#3190,#3191,#3192,#3193,#3194,
#3195,#3196,#3197,#3198));
#3272=CLOSED_SHELL('',(#3199,#3200,#3201,#3202,#3203,#3204,#3205,#3206,
#3207,#3208,#3209,#3210,#3211,#3212,#3213,#3214,#3215,#3216,#3217,#3218,
#3219,#3220));
#3273=CLOSED_SHELL('',(#3221,#3222,#3223,#3224,#3225,#3226,#3227,#3228,
#3229,#3230,#3231,#3232,#3233,#3234,#3235,#3236,#3237,#3238,#3239,#3240,
#3241,#3242,#3243,#3244,#3245,#3246,#3247,#3248,#3249,#3250));
#3274=CLOSED_SHELL('',(#3251,#3252,#3253,#3254,#3255,#3256,#3257,#3258,
#3259,#3260,#3261));
#3275=CLOSED_SHELL('',(#3262,#3263,#3264,#3265,#3266,#3267,#3268));
#3276=DERIVED_UNIT_ELEMENT(#3290,1.);
#3277=DERIVED_UNIT_ELEMENT(#5992,-3.);
#3278=DERIVED_UNIT_ELEMENT(#3290,1.);
#3279=DERIVED_UNIT_ELEMENT(#5992,-3.);
#3280=DERIVED_UNIT_ELEMENT(#3290,1.);
#3281=DERIVED_UNIT_ELEMENT(#5992,-3.);
#3282=DERIVED_UNIT_ELEMENT(#3290,1.);
#3283=DERIVED_UNIT_ELEMENT(#5992,-3.);
#3284=DERIVED_UNIT_ELEMENT(#3290,1.);
#3285=DERIVED_UNIT_ELEMENT(#5992,-3.);
#3286=DERIVED_UNIT_ELEMENT(#3290,1.);
#3287=DERIVED_UNIT_ELEMENT(#5992,-3.);
#3288=DERIVED_UNIT_ELEMENT(#3290,1.);
#3289=DERIVED_UNIT_ELEMENT(#5992,-3.);
#3290=(
MASS_UNIT()
NAMED_UNIT(*)
SI_UNIT(.KILO.,.GRAM.)
);
#3291=DERIVED_UNIT((#3276,#3277));
#3292=DERIVED_UNIT((#3278,#3279));
#3293=DERIVED_UNIT((#3280,#3281));
#3294=DERIVED_UNIT((#3282,#3283));
#3295=DERIVED_UNIT((#3284,#3285));
#3296=DERIVED_UNIT((#3286,#3287));
#3297=DERIVED_UNIT((#3288,#3289));
#3298=MEASURE_REPRESENTATION_ITEM('density measure',
POSITIVE_RATIO_MEASURE(7850.),#3291);
#3299=MEASURE_REPRESENTATION_ITEM('density measure',
POSITIVE_RATIO_MEASURE(7850.),#3292);
#3300=MEASURE_REPRESENTATION_ITEM('density measure',
POSITIVE_RATIO_MEASURE(7850.),#3293);
#3301=MEASURE_REPRESENTATION_ITEM('density measure',
POSITIVE_RATIO_MEASURE(7850.),#3294);
#3302=MEASURE_REPRESENTATION_ITEM('density measure',
POSITIVE_RATIO_MEASURE(7850.),#3295);
#3303=MEASURE_REPRESENTATION_ITEM('density measure',
POSITIVE_RATIO_MEASURE(7850.),#3296);
#3304=MEASURE_REPRESENTATION_ITEM('density measure',
POSITIVE_RATIO_MEASURE(7850.),#3297);
#3305=PROPERTY_DEFINITION_REPRESENTATION(#3340,#3319);
#3306=PROPERTY_DEFINITION_REPRESENTATION(#3341,#3320);
#3307=PROPERTY_DEFINITION_REPRESENTATION(#3342,#3321);
#3308=PROPERTY_DEFINITION_REPRESENTATION(#3343,#3322);
#3309=PROPERTY_DEFINITION_REPRESENTATION(#3344,#3323);
#3310=PROPERTY_DEFINITION_REPRESENTATION(#3345,#3324);
#3311=PROPERTY_DEFINITION_REPRESENTATION(#3346,#3325);
#3312=PROPERTY_DEFINITION_REPRESENTATION(#3347,#3326);
#3313=PROPERTY_DEFINITION_REPRESENTATION(#3348,#3327);
#3314=PROPERTY_DEFINITION_REPRESENTATION(#3349,#3328);
#3315=PROPERTY_DEFINITION_REPRESENTATION(#3350,#3329);
#3316=PROPERTY_DEFINITION_REPRESENTATION(#3351,#3330);
#3317=PROPERTY_DEFINITION_REPRESENTATION(#3352,#3331);
#3318=PROPERTY_DEFINITION_REPRESENTATION(#3353,#3332);
#3319=REPRESENTATION('material name',(#3333),#5983);
#3320=REPRESENTATION('density',(#3298),#5983);
#3321=REPRESENTATION('material name',(#3334),#5984);
#3322=REPRESENTATION('density',(#3299),#5984);
#3323=REPRESENTATION('material name',(#3335),#5985);
#3324=REPRESENTATION('density',(#3300),#5985);
#3325=REPRESENTATION('material name',(#3336),#5986);
#3326=REPRESENTATION('density',(#3301),#5986);
#3327=REPRESENTATION('material name',(#3337),#5987);
#3328=REPRESENTATION('density',(#3302),#5987);
#3329=REPRESENTATION('material name',(#3338),#5988);
#3330=REPRESENTATION('density',(#3303),#5988);
#3331=REPRESENTATION('material name',(#3339),#5989);
#3332=REPRESENTATION('density',(#3304),#5989);
#3333=DESCRIPTIVE_REPRESENTATION_ITEM('Steel','Steel');
#3334=DESCRIPTIVE_REPRESENTATION_ITEM('Steel','Steel');
#3335=DESCRIPTIVE_REPRESENTATION_ITEM('Steel','Steel');
#3336=DESCRIPTIVE_REPRESENTATION_ITEM('Steel','Steel');
#3337=DESCRIPTIVE_REPRESENTATION_ITEM('Steel','Steel');
#3338=DESCRIPTIVE_REPRESENTATION_ITEM('Steel','Steel');
#3339=DESCRIPTIVE_REPRESENTATION_ITEM('Steel','Steel');
#3340=PROPERTY_DEFINITION('material property','material name',#6030);
#3341=PROPERTY_DEFINITION('material property','density of part',#6030);
#3342=PROPERTY_DEFINITION('material property','material name',#6031);
#3343=PROPERTY_DEFINITION('material property','density of part',#6031);
#3344=PROPERTY_DEFINITION('material property','material name',#6032);
#3345=PROPERTY_DEFINITION('material property','density of part',#6032);
#3346=PROPERTY_DEFINITION('material property','material name',#6033);
#3347=PROPERTY_DEFINITION('material property','density of part',#6033);
#3348=PROPERTY_DEFINITION('material property','material name',#6034);
#3349=PROPERTY_DEFINITION('material property','density of part',#6034);
#3350=PROPERTY_DEFINITION('material property','material name',#6035);
#3351=PROPERTY_DEFINITION('material property','density of part',#6035);
#3352=PROPERTY_DEFINITION('material property','material name',#6036);
#3353=PROPERTY_DEFINITION('material property','density of part',#6036);
#3354=AXIS2_PLACEMENT_3D('',#4650,#3685,#3686);
#3355=AXIS2_PLACEMENT_3D('',#4651,#3687,#3688);
#3356=AXIS2_PLACEMENT_3D('',#4652,#3689,#3690);
#3357=AXIS2_PLACEMENT_3D('',#4654,#3691,#3692);
#3358=AXIS2_PLACEMENT_3D('',#4657,#3694,#3695);
#3359=AXIS2_PLACEMENT_3D('',#4658,#3696,#3697);
#3360=AXIS2_PLACEMENT_3D('',#4660,#3698,#3699);
#3361=AXIS2_PLACEMENT_3D('',#4663,#3701,#3702);
#3362=AXIS2_PLACEMENT_3D('',#4664,#3703,#3704);
#3363=AXIS2_PLACEMENT_3D('',#4666,#3705,#3706);
#3364=AXIS2_PLACEMENT_3D('',#4669,#3708,#3709);
#3365=AXIS2_PLACEMENT_3D('',#4670,#3710,#3711);
#3366=AXIS2_PLACEMENT_3D('',#4672,#3712,#3713);
#3367=AXIS2_PLACEMENT_3D('',#4675,#3715,#3716);
#3368=AXIS2_PLACEMENT_3D('',#4676,#3717,#3718);
#3369=AXIS2_PLACEMENT_3D('',#4685,#3723,#3724);
#3370=AXIS2_PLACEMENT_3D('',#4694,#3729,#3730);
#3371=AXIS2_PLACEMENT_3D('',#4699,#3732,#3733);
#3372=AXIS2_PLACEMENT_3D('',#4711,#3739,#3740);
#3373=AXIS2_PLACEMENT_3D('',#4715,#3742,#3743);
#3374=AXIS2_PLACEMENT_3D('',#4719,#3745,#3746);
#3375=AXIS2_PLACEMENT_3D('',#4723,#3748,#3749);
#3376=AXIS2_PLACEMENT_3D('',#4727,#3751,#3752);
#3377=AXIS2_PLACEMENT_3D('',#4731,#3754,#3755);
#3378=AXIS2_PLACEMENT_3D('',#4735,#3757,#3758);
#3379=AXIS2_PLACEMENT_3D('',#4739,#3760,#3761);
#3380=AXIS2_PLACEMENT_3D('',#4743,#3763,#3764);
#3381=AXIS2_PLACEMENT_3D('',#4754,#3770,#3771);
#3382=AXIS2_PLACEMENT_3D('',#4755,#3772,#3773);
#3383=AXIS2_PLACEMENT_3D('',#4758,#3775,#3776);
#3384=AXIS2_PLACEMENT_3D('',#4760,#3777,#3778);
#3385=AXIS2_PLACEMENT_3D('',#4772,#3784,#3785);
#3386=AXIS2_PLACEMENT_3D('',#4776,#3787,#3788);
#3387=AXIS2_PLACEMENT_3D('',#4780,#3790,#3791);
#3388=AXIS2_PLACEMENT_3D('',#4784,#3793,#3794);
#3389=AXIS2_PLACEMENT_3D('',#4788,#3796,#3797);
#3390=AXIS2_PLACEMENT_3D('',#4792,#3799,#3800);
#3391=AXIS2_PLACEMENT_3D('',#4796,#3802,#3803);
#3392=AXIS2_PLACEMENT_3D('',#4800,#3805,#3806);
#3393=AXIS2_PLACEMENT_3D('',#4804,#3808,#3809);
#3394=AXIS2_PLACEMENT_3D('',#4810,#3813,#3814);
#3395=AXIS2_PLACEMENT_3D('',#4813,#3817,#3818);
#3396=AXIS2_PLACEMENT_3D('',#4816,#3821,#3822);
#3397=AXIS2_PLACEMENT_3D('',#4819,#3825,#3826);
#3398=AXIS2_PLACEMENT_3D('',#4822,#3829,#3830);
#3399=AXIS2_PLACEMENT_3D('',#4825,#3833,#3834);
#3400=AXIS2_PLACEMENT_3D('',#4828,#3837,#3838);
#3401=AXIS2_PLACEMENT_3D('',#4831,#3841,#3842);
#3402=AXIS2_PLACEMENT_3D('',#4834,#3845,#3846);
#3403=AXIS2_PLACEMENT_3D('',#4837,#3849,#3850);
#3404=AXIS2_PLACEMENT_3D('',#4842,#3854,#3855);
#3405=AXIS2_PLACEMENT_3D('',#4846,#3858,#3859);
#3406=AXIS2_PLACEMENT_3D('',#4849,#3862,#3863);
#3407=AXIS2_PLACEMENT_3D('',#4851,#3865,#3866);
#3408=AXIS2_PLACEMENT_3D('',#4861,#3872,#3873);
#3409=AXIS2_PLACEMENT_3D('',#4872,#3880,#3881);
#3410=AXIS2_PLACEMENT_3D('',#4878,#3885,#3886);
#3411=AXIS2_PLACEMENT_3D('',#4889,#3893,#3894);
#3412=AXIS2_PLACEMENT_3D('',#4890,#3895,#3896);
#3413=AXIS2_PLACEMENT_3D('',#4892,#3898,#3899);
#3414=AXIS2_PLACEMENT_3D('',#4893,#3900,#3901);
#3415=AXIS2_PLACEMENT_3D('',#4894,#3902,#3903);
#3416=AXIS2_PLACEMENT_3D('',#4895,#3904,#3905);
#3417=AXIS2_PLACEMENT_3D('',#4896,#3906,#3907);
#3418=AXIS2_PLACEMENT_3D('',#4897,#3908,#3909);
#3419=AXIS2_PLACEMENT_3D('',#4898,#3910,#3911);
#3420=AXIS2_PLACEMENT_3D('',#4899,#3912,#3913);
#3421=AXIS2_PLACEMENT_3D('',#4900,#3914,#3915);
#3422=AXIS2_PLACEMENT_3D('',#4901,#3916,#3917);
#3423=AXIS2_PLACEMENT_3D('',#4904,#3920,#3921);
#3424=AXIS2_PLACEMENT_3D('',#4907,#3924,#3925);
#3425=AXIS2_PLACEMENT_3D('',#4908,#3926,#3927);
#3426=AXIS2_PLACEMENT_3D('',#4909,#3928,#3929);
#3427=AXIS2_PLACEMENT_3D('',#4910,#3930,#3931);
#3428=AXIS2_PLACEMENT_3D('',#4911,#3932,#3933);
#3429=AXIS2_PLACEMENT_3D('',#4913,#3935,#3936);
#3430=AXIS2_PLACEMENT_3D('',#4914,#3937,#3938);
#3431=AXIS2_PLACEMENT_3D('',#4916,#3940,#3941);
#3432=AXIS2_PLACEMENT_3D('',#4917,#3942,#3943);
#3433=AXIS2_PLACEMENT_3D('',#4918,#3944,#3945);
#3434=AXIS2_PLACEMENT_3D('',#4919,#3946,#3947);
#3435=AXIS2_PLACEMENT_3D('',#4920,#3948,#3949);
#3436=AXIS2_PLACEMENT_3D('',#4921,#3950,#3951);
#3437=AXIS2_PLACEMENT_3D('',#4922,#3952,#3953);
#3438=AXIS2_PLACEMENT_3D('',#4923,#3954,#3955);
#3439=AXIS2_PLACEMENT_3D('',#4925,#3956,#3957);
#3440=AXIS2_PLACEMENT_3D('',#4928,#3959,#3960);
#3441=AXIS2_PLACEMENT_3D('',#4929,#3961,#3962);
#3442=AXIS2_PLACEMENT_3D('',#4931,#3963,#3964);
#3443=AXIS2_PLACEMENT_3D('',#4934,#3966,#3967);
#3444=AXIS2_PLACEMENT_3D('',#4935,#3968,#3969);
#3445=AXIS2_PLACEMENT_3D('',#4937,#3970,#3971);
#3446=AXIS2_PLACEMENT_3D('',#4940,#3973,#3974);
#3447=AXIS2_PLACEMENT_3D('',#4941,#3975,#3976);
#3448=AXIS2_PLACEMENT_3D('',#4946,#3978,#3979);
#3449=AXIS2_PLACEMENT_3D('',#4950,#3981,#3982);
#3450=AXIS2_PLACEMENT_3D('',#4954,#3985,#3986);
#3451=AXIS2_PLACEMENT_3D('',#4960,#3990,#3991);
#3452=AXIS2_PLACEMENT_3D('',#4977,#4000,#4001);
#3453=AXIS2_PLACEMENT_3D('',#4987,#4006,#4007);
#3454=AXIS2_PLACEMENT_3D('',#4991,#4009,#4010);
#3455=AXIS2_PLACEMENT_3D('',#4995,#4012,#4013);
#3456=AXIS2_PLACEMENT_3D('',#4999,#4015,#4016);
#3457=AXIS2_PLACEMENT_3D('',#5003,#4018,#4019);
#3458=AXIS2_PLACEMENT_3D('',#5007,#4021,#4022);
#3459=AXIS2_PLACEMENT_3D('',#5011,#4024,#4025);
#3460=AXIS2_PLACEMENT_3D('',#5015,#4027,#4028);
#3461=AXIS2_PLACEMENT_3D('',#5019,#4030,#4031);
#3462=AXIS2_PLACEMENT_3D('',#5025,#4035,#4036);
#3463=AXIS2_PLACEMENT_3D('',#5030,#4038,#4039);
#3464=AXIS2_PLACEMENT_3D('',#5037,#4043,#4044);
#3465=AXIS2_PLACEMENT_3D('',#5038,#4045,#4046);
#3466=AXIS2_PLACEMENT_3D('',#5047,#4051,#4052);
#3467=AXIS2_PLACEMENT_3D('',#5057,#4057,#4058);
#3468=AXIS2_PLACEMENT_3D('',#5061,#4060,#4061);
#3469=AXIS2_PLACEMENT_3D('',#5065,#4063,#4064);
#3470=AXIS2_PLACEMENT_3D('',#5069,#4066,#4067);
#3471=AXIS2_PLACEMENT_3D('',#5073,#4069,#4070);
#3472=AXIS2_PLACEMENT_3D('',#5077,#4072,#4073);
#3473=AXIS2_PLACEMENT_3D('',#5081,#4075,#4076);
#3474=AXIS2_PLACEMENT_3D('',#5085,#4078,#4079);
#3475=AXIS2_PLACEMENT_3D('',#5089,#4081,#4082);
#3476=AXIS2_PLACEMENT_3D('',#5095,#4086,#4087);
#3477=AXIS2_PLACEMENT_3D('',#5098,#4090,#4091);
#3478=AXIS2_PLACEMENT_3D('',#5101,#4094,#4095);
#3479=AXIS2_PLACEMENT_3D('',#5104,#4098,#4099);
#3480=AXIS2_PLACEMENT_3D('',#5107,#4102,#4103);
#3481=AXIS2_PLACEMENT_3D('',#5110,#4106,#4107);
#3482=AXIS2_PLACEMENT_3D('',#5113,#4110,#4111);
#3483=AXIS2_PLACEMENT_3D('',#5116,#4114,#4115);
#3484=AXIS2_PLACEMENT_3D('',#5119,#4118,#4119);
#3485=AXIS2_PLACEMENT_3D('',#5122,#4122,#4123);
#3486=AXIS2_PLACEMENT_3D('',#5126,#4127,#4128);
#3487=AXIS2_PLACEMENT_3D('',#5129,#4131,#4132);
#3488=AXIS2_PLACEMENT_3D('',#5130,#4133,#4134);
#3489=AXIS2_PLACEMENT_3D('',#5142,#4142,#4143);
#3490=AXIS2_PLACEMENT_3D('',#5148,#4147,#4148);
#3491=AXIS2_PLACEMENT_3D('',#5160,#4156,#4157);
#3492=AXIS2_PLACEMENT_3D('',#5161,#4158,#4159);
#3493=AXIS2_PLACEMENT_3D('',#5163,#4161,#4162);
#3494=AXIS2_PLACEMENT_3D('',#5164,#4163,#4164);
#3495=AXIS2_PLACEMENT_3D('',#5165,#4165,#4166);
#3496=AXIS2_PLACEMENT_3D('',#5166,#4167,#4168);
#3497=AXIS2_PLACEMENT_3D('',#5167,#4169,#4170);
#3498=AXIS2_PLACEMENT_3D('',#5168,#4171,#4172);
#3499=AXIS2_PLACEMENT_3D('',#5169,#4173,#4174);
#3500=AXIS2_PLACEMENT_3D('',#5170,#4175,#4176);
#3501=AXIS2_PLACEMENT_3D('',#5171,#4177,#4178);
#3502=AXIS2_PLACEMENT_3D('',#5172,#4179,#4180);
#3503=AXIS2_PLACEMENT_3D('',#5174,#4182,#4183);
#3504=AXIS2_PLACEMENT_3D('',#5176,#4185,#4186);
#3505=AXIS2_PLACEMENT_3D('',#5177,#4187,#4188);
#3506=AXIS2_PLACEMENT_3D('',#5179,#4190,#4191);
#3507=AXIS2_PLACEMENT_3D('',#5181,#4193,#4194);
#3508=AXIS2_PLACEMENT_3D('',#5182,#4195,#4196);
#3509=AXIS2_PLACEMENT_3D('',#5183,#4197,#4198);
#3510=AXIS2_PLACEMENT_3D('',#5184,#4199,#4200);
#3511=AXIS2_PLACEMENT_3D('',#5186,#4202,#4203);
#3512=AXIS2_PLACEMENT_3D('',#5187,#4204,#4205);
#3513=AXIS2_PLACEMENT_3D('',#5189,#4207,#4208);
#3514=AXIS2_PLACEMENT_3D('',#5190,#4209,#4210);
#3515=AXIS2_PLACEMENT_3D('',#5191,#4211,#4212);
#3516=AXIS2_PLACEMENT_3D('',#5192,#4213,#4214);
#3517=AXIS2_PLACEMENT_3D('',#5193,#4215,#4216);
#3518=AXIS2_PLACEMENT_3D('',#5194,#4217,#4218);
#3519=AXIS2_PLACEMENT_3D('',#5195,#4219,#4220);
#3520=AXIS2_PLACEMENT_3D('',#5196,#4221,#4222);
#3521=AXIS2_PLACEMENT_3D('',#5198,#4223,#4224);
#3522=AXIS2_PLACEMENT_3D('',#5201,#4226,#4227);
#3523=AXIS2_PLACEMENT_3D('',#5202,#4228,#4229);
#3524=AXIS2_PLACEMENT_3D('',#5217,#4233,#4234);
#3525=AXIS2_PLACEMENT_3D('',#5228,#4240,#4241);
#3526=AXIS2_PLACEMENT_3D('',#5229,#4242,#4243);
#3527=AXIS2_PLACEMENT_3D('',#5232,#4245,#4246);
#3528=AXIS2_PLACEMENT_3D('',#5233,#4247,#4248);
#3529=AXIS2_PLACEMENT_3D('',#5234,#4249,#4250);
#3530=AXIS2_PLACEMENT_3D('',#5236,#4251,#4252);
#3531=AXIS2_PLACEMENT_3D('',#5238,#4254,#4255);
#3532=AXIS2_PLACEMENT_3D('',#5240,#4256,#4257);
#3533=AXIS2_PLACEMENT_3D('',#5242,#4259,#4260);
#3534=AXIS2_PLACEMENT_3D('',#5246,#4263,#4264);
#3535=AXIS2_PLACEMENT_3D('',#5248,#4266,#4267);
#3536=AXIS2_PLACEMENT_3D('',#5249,#4268,#4269);
#3537=AXIS2_PLACEMENT_3D('',#5250,#4270,#4271);
#3538=AXIS2_PLACEMENT_3D('',#5252,#4273,#4274);
#3539=AXIS2_PLACEMENT_3D('',#5253,#4275,#4276);
#3540=AXIS2_PLACEMENT_3D('',#5254,#4277,#4278);
#3541=AXIS2_PLACEMENT_3D('',#5255,#4279,#4280);
#3542=AXIS2_PLACEMENT_3D('',#5257,#4281,#4282);
#3543=AXIS2_PLACEMENT_3D('',#5260,#4284,#4285);
#3544=AXIS2_PLACEMENT_3D('',#5261,#4286,#4287);
#3545=AXIS2_PLACEMENT_3D('',#5300,#4288,#4289);
#3546=AXIS2_PLACEMENT_3D('',#5303,#4290,#4291);
#3547=AXIS2_PLACEMENT_3D('',#5304,#4292,#4293);
#3548=AXIS2_PLACEMENT_3D('',#5305,#4294,#4295);
#3549=AXIS2_PLACEMENT_3D('',#5308,#4296,#4297);
#3550=AXIS2_PLACEMENT_3D('',#5309,#4298,#4299);
#3551=AXIS2_PLACEMENT_3D('',#5310,#4300,#4301);
#3552=AXIS2_PLACEMENT_3D('',#5313,#4302,#4303);
#3553=AXIS2_PLACEMENT_3D('',#5314,#4304,#4305);
#3554=AXIS2_PLACEMENT_3D('',#5315,#4306,#4307);
#3555=AXIS2_PLACEMENT_3D('',#5318,#4308,#4309);
#3556=AXIS2_PLACEMENT_3D('',#5319,#4310,#4311);
#3557=AXIS2_PLACEMENT_3D('',#5320,#4312,#4313);
#3558=AXIS2_PLACEMENT_3D('',#5337,#4314,#4315);
#3559=AXIS2_PLACEMENT_3D('',#5339,#4316,#4317);
#3560=AXIS2_PLACEMENT_3D('',#5353,#4318,#4319);
#3561=AXIS2_PLACEMENT_3D('',#5402,#4320,#4321);
#3562=AXIS2_PLACEMENT_3D('',#5451,#4322,#4323);
#3563=AXIS2_PLACEMENT_3D('',#5500,#4324,#4325);
#3564=AXIS2_PLACEMENT_3D('',#5515,#4329,#4330);
#3565=AXIS2_PLACEMENT_3D('',#5528,#4337,#4338);
#3566=AXIS2_PLACEMENT_3D('',#5529,#4339,#4340);
#3567=AXIS2_PLACEMENT_3D('',#5532,#4342,#4343);
#3568=AXIS2_PLACEMENT_3D('',#5533,#4344,#4345);
#3569=AXIS2_PLACEMENT_3D('',#5534,#4346,#4347);
#3570=AXIS2_PLACEMENT_3D('',#5536,#4348,#4349);
#3571=AXIS2_PLACEMENT_3D('',#5538,#4351,#4352);
#3572=AXIS2_PLACEMENT_3D('',#5539,#4353,#4354);
#3573=AXIS2_PLACEMENT_3D('',#5542,#4356,#4357);
#3574=AXIS2_PLACEMENT_3D('',#5543,#4358,#4359);
#3575=AXIS2_PLACEMENT_3D('',#5550,#4366,#4367);
#3576=AXIS2_PLACEMENT_3D('',#5552,#4369,#4370);
#3577=AXIS2_PLACEMENT_3D('',#5566,#4371,#4372);
#3578=AXIS2_PLACEMENT_3D('',#5567,#4373,#4374);
#3579=AXIS2_PLACEMENT_3D('',#5568,#4375,#4376);
#3580=AXIS2_PLACEMENT_3D('',#5569,#4377,#4378);
#3581=AXIS2_PLACEMENT_3D('',#5570,#4379,#4380);
#3582=AXIS2_PLACEMENT_3D('',#5572,#4382,#4383);
#3583=AXIS2_PLACEMENT_3D('',#5585,#4384,#4385);
#3584=AXIS2_PLACEMENT_3D('',#5586,#4386,#4387);
#3585=AXIS2_PLACEMENT_3D('',#5587,#4388,#4389);
#3586=AXIS2_PLACEMENT_3D('',#5588,#4390,#4391);
#3587=AXIS2_PLACEMENT_3D('',#5590,#4392,#4393);
#3588=AXIS2_PLACEMENT_3D('',#5593,#4395,#4396);
#3589=AXIS2_PLACEMENT_3D('',#5594,#4397,#4398);
#3590=AXIS2_PLACEMENT_3D('',#5597,#4399,#4400);
#3591=AXIS2_PLACEMENT_3D('',#5599,#4401,#4402);
#3592=AXIS2_PLACEMENT_3D('',#5601,#4403,#4404);
#3593=AXIS2_PLACEMENT_3D('',#5605,#4406,#4407);
#3594=AXIS2_PLACEMENT_3D('',#5607,#4408,#4409);
#3595=AXIS2_PLACEMENT_3D('',#5609,#4410,#4411);
#3596=AXIS2_PLACEMENT_3D('',#5611,#4412,#4413);
#3597=AXIS2_PLACEMENT_3D('',#5613,#4414,#4415);
#3598=AXIS2_PLACEMENT_3D('',#5614,#4416,#4417);
#3599=AXIS2_PLACEMENT_3D('',#5616,#4418,#4419);
#3600=AXIS2_PLACEMENT_3D('',#5618,#4420,#4421);
#3601=AXIS2_PLACEMENT_3D('',#5619,#4422,#4423);
#3602=AXIS2_PLACEMENT_3D('',#5620,#4424,#4425);
#3603=AXIS2_PLACEMENT_3D('',#5624,#4428,#4429);
#3604=AXIS2_PLACEMENT_3D('',#5628,#4432,#4433);
#3605=AXIS2_PLACEMENT_3D('',#5632,#4436,#4437);
#3606=AXIS2_PLACEMENT_3D('',#5669,#4443,#4444);
#3607=AXIS2_PLACEMENT_3D('',#5706,#4450,#4451);
#3608=AXIS2_PLACEMENT_3D('',#5710,#4454,#4455);
#3609=AXIS2_PLACEMENT_3D('',#5711,#4456,#4457);
#3610=AXIS2_PLACEMENT_3D('',#5712,#4458,#4459);
#3611=AXIS2_PLACEMENT_3D('',#5713,#4460,#4461);
#3612=AXIS2_PLACEMENT_3D('',#5714,#4462,#4463);
#3613=AXIS2_PLACEMENT_3D('',#5715,#4464,#4465);
#3614=AXIS2_PLACEMENT_3D('',#5716,#4466,#4467);
#3615=AXIS2_PLACEMENT_3D('',#5717,#4468,#4469);
#3616=AXIS2_PLACEMENT_3D('',#5718,#4470,#4471);
#3617=AXIS2_PLACEMENT_3D('',#5728,#4477,#4478);
#3618=AXIS2_PLACEMENT_3D('',#5735,#4483,#4484);
#3619=AXIS2_PLACEMENT_3D('',#5742,#4489,#4490);
#3620=AXIS2_PLACEMENT_3D('',#5749,#4495,#4496);
#3621=AXIS2_PLACEMENT_3D('',#5756,#4501,#4502);
#3622=AXIS2_PLACEMENT_3D('',#5760,#4506,#4507);
#3623=AXIS2_PLACEMENT_3D('',#5761,#4508,#4509);
#3624=AXIS2_PLACEMENT_3D('',#5762,#4510,#4511);
#3625=AXIS2_PLACEMENT_3D('',#5763,#4512,#4513);
#3626=AXIS2_PLACEMENT_3D('',#5764,#4514,#4515);
#3627=AXIS2_PLACEMENT_3D('',#5765,#4516,#4517);
#3628=AXIS2_PLACEMENT_3D('',#5766,#4518,#4519);
#3629=AXIS2_PLACEMENT_3D('',#5767,#4520,#4521);
#3630=AXIS2_PLACEMENT_3D('',#5768,#4522,#4523);
#3631=AXIS2_PLACEMENT_3D('',#5823,#4524,#4525);
#3632=AXIS2_PLACEMENT_3D('',#5824,#4526,#4527);
#3633=AXIS2_PLACEMENT_3D('',#5825,#4528,#4529);
#3634=AXIS2_PLACEMENT_3D('',#5826,#4530,#4531);
#3635=AXIS2_PLACEMENT_3D('',#5881,#4532,#4533);
#3636=AXIS2_PLACEMENT_3D('',#5882,#4534,#4535);
#3637=AXIS2_PLACEMENT_3D('',#5883,#4536,#4537);
#3638=AXIS2_PLACEMENT_3D('',#5884,#4538,#4539);
#3639=AXIS2_PLACEMENT_3D('',#5885,#4540,#4541);
#3640=AXIS2_PLACEMENT_3D('',#5887,#4542,#4543);
#3641=AXIS2_PLACEMENT_3D('',#5890,#4545,#4546);
#3642=AXIS2_PLACEMENT_3D('',#5891,#4547,#4548);
#3643=AXIS2_PLACEMENT_3D('',#5894,#4549,#4550);
#3644=AXIS2_PLACEMENT_3D('',#5898,#4552,#4553);
#3645=AXIS2_PLACEMENT_3D('',#5900,#4555,#4556);
#3646=AXIS2_PLACEMENT_3D('',#5903,#4557,#4558);
#3647=AXIS2_PLACEMENT_3D('',#5907,#4560,#4561);
#3648=AXIS2_PLACEMENT_3D('',#5909,#4563,#4564);
#3649=AXIS2_PLACEMENT_3D('',#5914,#4566,#4567);
#3650=AXIS2_PLACEMENT_3D('',#5917,#4569,#4570);
#3651=AXIS2_PLACEMENT_3D('',#5919,#4572,#4573);
#3652=AXIS2_PLACEMENT_3D('',#5920,#4574,#4575);
#3653=AXIS2_PLACEMENT_3D('',#5923,#4576,#4577);
#3654=AXIS2_PLACEMENT_3D('',#5926,#4579,#4580);
#3655=AXIS2_PLACEMENT_3D('',#5929,#4582,#4583);
#3656=AXIS2_PLACEMENT_3D('',#5931,#4585,#4586);
#3657=AXIS2_PLACEMENT_3D('',#5932,#4587,#4588);
#3658=AXIS2_PLACEMENT_3D('',#5935,#4591,#4592);
#3659=AXIS2_PLACEMENT_3D('',#5938,#4595,#4596);
#3660=AXIS2_PLACEMENT_3D('',#5939,#4597,#4598);
#3661=AXIS2_PLACEMENT_3D('',#5940,#4599,#4600);
#3662=AXIS2_PLACEMENT_3D('',#5941,#4601,#4602);
#3663=AXIS2_PLACEMENT_3D('',#5942,#4603,#4604);
#3664=AXIS2_PLACEMENT_3D('',#5944,#4605,#4606);
#3665=AXIS2_PLACEMENT_3D('',#5947,#4608,#4609);
#3666=AXIS2_PLACEMENT_3D('',#5948,#4610,#4611);
#3667=AXIS2_PLACEMENT_3D('',#5950,#4612,#4613);
#3668=AXIS2_PLACEMENT_3D('',#5953,#4615,#4616);
#3669=AXIS2_PLACEMENT_3D('',#5954,#4617,#4618);
#3670=AXIS2_PLACEMENT_3D('',#5956,#4619,#4620);
#3671=AXIS2_PLACEMENT_3D('',#5959,#4622,#4623);
#3672=AXIS2_PLACEMENT_3D('',#5960,#4624,#4625);
#3673=AXIS2_PLACEMENT_3D('',#5961,#4626,#4627);
#3674=AXIS2_PLACEMENT_3D('',#5962,#4628,#4629);
#3675=AXIS2_PLACEMENT_3D('',#5963,#4630,#4631);
#3676=AXIS2_PLACEMENT_3D('',#5964,#4632,#4633);
#3677=AXIS2_PLACEMENT_3D('',#5965,#4634,#4635);
#3678=AXIS2_PLACEMENT_3D('',#5966,#4636,#4637);
#3679=AXIS2_PLACEMENT_3D('',#5967,#4638,#4639);
#3680=AXIS2_PLACEMENT_3D('',#5968,#4640,#4641);
#3681=AXIS2_PLACEMENT_3D('',#5969,#4642,#4643);
#3682=AXIS2_PLACEMENT_3D('',#5970,#4644,#4645);
#3683=AXIS2_PLACEMENT_3D('',#5971,#4646,#4647);
#3684=AXIS2_PLACEMENT_3D('',#5972,#4648,#4649);
#3685=DIRECTION('axis',(0.,0.,1.));
#3686=DIRECTION('refdir',(1.,0.,0.));
#3687=DIRECTION('axis',(0.,0.,1.));
#3688=DIRECTION('refdir',(1.,0.,0.));
#3689=DIRECTION('center_axis',(0.,0.,-1.));
#3690=DIRECTION('ref_axis',(-1.,0.,0.));
#3691=DIRECTION('center_axis',(0.,0.,-1.));
#3692=DIRECTION('ref_axis',(-1.,0.,0.));
#3693=DIRECTION('',(0.,0.,-1.));
#3694=DIRECTION('center_axis',(5.55111512312578E-17,2.47817639425258E-17,
1.));
#3695=DIRECTION('ref_axis',(1.,-1.37566424599088E-33,-5.55111512312578E-17));
#3696=DIRECTION('center_axis',(0.,0.,-1.));
#3697=DIRECTION('ref_axis',(-1.,0.,0.));
#3698=DIRECTION('center_axis',(5.55111512312578E-17,2.47817639425258E-17,
1.));
#3699=DIRECTION('ref_axis',(1.,-1.37566424599088E-33,-5.55111512312578E-17));
#3700=DIRECTION('',(0.,0.,-1.));
#3701=DIRECTION('center_axis',(0.,0.,-1.));
#3702=DIRECTION('ref_axis',(-1.,0.,0.));
#3703=DIRECTION('center_axis',(0.,0.,1.));
#3704=DIRECTION('ref_axis',(1.,0.,0.));
#3705=DIRECTION('center_axis',(0.,0.,1.));
#3706=DIRECTION('ref_axis',(1.,0.,0.));
#3707=DIRECTION('',(0.,0.,1.));
#3708=DIRECTION('center_axis',(0.,0.,1.));
#3709=DIRECTION('ref_axis',(1.,0.,0.));
#3710=DIRECTION('center_axis',(0.,0.,1.));
#3711=DIRECTION('ref_axis',(1.,0.,0.));
#3712=DIRECTION('center_axis',(0.,0.,1.));
#3713=DIRECTION('ref_axis',(1.,0.,0.));
#3714=DIRECTION('',(0.,0.,1.));
#3715=DIRECTION('center_axis',(0.,0.,1.));
#3716=DIRECTION('ref_axis',(1.,0.,0.));
#3717=DIRECTION('center_axis',(0.,1.,0.));
#3718=DIRECTION('ref_axis',(0.,0.,1.));
#3719=DIRECTION('',(1.,0.,0.));
#3720=DIRECTION('',(0.,0.,1.));
#3721=DIRECTION('',(-1.,1.79745021839835E-17,5.55111512312578E-17));
#3722=DIRECTION('',(0.,0.,-1.));
#3723=DIRECTION('center_axis',(-0.766044443118972,-0.642787609686546,0.));
#3724=DIRECTION('ref_axis',(0.642787609686546,-0.766044443118972,0.));
#3725=DIRECTION('',(-0.642787609686546,0.766044443118972,0.));
#3726=DIRECTION('',(0.,0.,-1.));
#3727=DIRECTION('',(-0.642787609686546,0.766044443118972,0.));
#3728=DIRECTION('',(0.,0.,-1.));
#3729=DIRECTION('center_axis',(0.,0.,-1.));
#3730=DIRECTION('ref_axis',(-1.,0.,0.));
#3731=DIRECTION('',(1.,0.,0.));
#3732=DIRECTION('center_axis',(0.,0.,1.));
#3733=DIRECTION('ref_axis',(-1.,0.,0.));
#3734=DIRECTION('',(-8.47613560090905E-17,1.,0.));
#3735=DIRECTION('',(-0.642787609686546,0.766044443118972,0.));
#3736=DIRECTION('',(0.,1.,0.));
#3737=DIRECTION('',(1.,0.,0.));
#3738=DIRECTION('',(-1.23908819712629E-16,1.,0.));
#3739=DIRECTION('center_axis',(0.,0.,1.));
#3740=DIRECTION('ref_axis',(1.,0.,0.));
#3741=DIRECTION('',(-1.23908819712629E-16,1.,0.));
#3742=DIRECTION('center_axis',(0.,0.,1.));
#3743=DIRECTION('ref_axis',(1.,0.,0.));
#3744=DIRECTION('',(-1.23908819712629E-16,1.,0.));
#3745=DIRECTION('center_axis',(0.,0.,1.));
#3746=DIRECTION('ref_axis',(1.,0.,0.));
#3747=DIRECTION('',(-1.23908819712629E-16,1.,0.));
#3748=DIRECTION('center_axis',(0.,0.,1.));
#3749=DIRECTION('ref_axis',(1.,0.,0.));
#3750=DIRECTION('',(-1.23908819712629E-16,1.,0.));
#3751=DIRECTION('center_axis',(0.,0.,1.));
#3752=DIRECTION('ref_axis',(1.,0.,0.));
#3753=DIRECTION('',(-1.23908819712629E-16,1.,0.));
#3754=DIRECTION('center_axis',(0.,0.,1.));
#3755=DIRECTION('ref_axis',(1.,0.,0.));
#3756=DIRECTION('',(-1.23908819712629E-16,1.,0.));
#3757=DIRECTION('center_axis',(0.,0.,1.));
#3758=DIRECTION('ref_axis',(1.,0.,0.));
#3759=DIRECTION('',(-1.23908819712629E-16,1.,0.));
#3760=DIRECTION('center_axis',(0.,0.,1.));
#3761=DIRECTION('ref_axis',(1.,0.,0.));
#3762=DIRECTION('',(-1.23908819712629E-16,1.,0.));
#3763=DIRECTION('center_axis',(0.,0.,1.));
#3764=DIRECTION('ref_axis',(1.,0.,0.));
#3765=DIRECTION('',(-1.23908819712629E-16,1.,0.));
#3766=DIRECTION('',(-1.,0.,0.));
#3767=DIRECTION('',(-0.258819045102514,-0.96592582628907,0.));
#3768=DIRECTION('',(0.642787609686546,-0.766044443118972,0.));
#3769=DIRECTION('',(-4.47692281884469E-17,-1.,0.));
#3770=DIRECTION('center_axis',(0.,0.,1.));
#3771=DIRECTION('ref_axis',(-1.,0.,0.));
#3772=DIRECTION('center_axis',(0.,0.,-1.));
#3773=DIRECTION('ref_axis',(-1.,0.,0.));
#3774=DIRECTION('',(-8.47613560090905E-17,1.,0.));
#3775=DIRECTION('center_axis',(0.,0.,-1.));
#3776=DIRECTION('ref_axis',(-1.,0.,0.));
#3777=DIRECTION('center_axis',(0.,0.,-1.));
#3778=DIRECTION('ref_axis',(-1.,0.,0.));
#3779=DIRECTION('',(-4.47692281884469E-17,-1.,0.));
#3780=DIRECTION('',(0.642787609686546,-0.766044443118972,0.));
#3781=DIRECTION('',(-0.258819045102514,-0.96592582628907,0.));
#3782=DIRECTION('',(-1.,0.,0.));
#3783=DIRECTION('',(-1.23908819712629E-16,1.,0.));
#3784=DIRECTION('center_axis',(0.,0.,1.));
#3785=DIRECTION('ref_axis',(1.,0.,0.));
#3786=DIRECTION('',(-1.23908819712629E-16,1.,0.));
#3787=DIRECTION('center_axis',(0.,0.,1.));
#3788=DIRECTION('ref_axis',(1.,0.,0.));
#3789=DIRECTION('',(-1.23908819712629E-16,1.,0.));
#3790=DIRECTION('center_axis',(0.,0.,1.));
#3791=DIRECTION('ref_axis',(1.,0.,0.));
#3792=DIRECTION('',(-1.23908819712629E-16,1.,0.));
#3793=DIRECTION('center_axis',(0.,0.,1.));
#3794=DIRECTION('ref_axis',(1.,0.,0.));
#3795=DIRECTION('',(-1.23908819712629E-16,1.,0.));
#3796=DIRECTION('center_axis',(0.,0.,1.));
#3797=DIRECTION('ref_axis',(1.,0.,0.));
#3798=DIRECTION('',(-1.23908819712629E-16,1.,0.));
#3799=DIRECTION('center_axis',(0.,0.,1.));
#3800=DIRECTION('ref_axis',(1.,0.,0.));
#3801=DIRECTION('',(-1.23908819712629E-16,1.,0.));
#3802=DIRECTION('center_axis',(0.,0.,1.));
#3803=DIRECTION('ref_axis',(1.,0.,0.));
#3804=DIRECTION('',(-1.23908819712629E-16,1.,0.));
#3805=DIRECTION('center_axis',(0.,0.,1.));
#3806=DIRECTION('ref_axis',(1.,0.,0.));
#3807=DIRECTION('',(-1.23908819712629E-16,1.,0.));
#3808=DIRECTION('center_axis',(0.,0.,1.));
#3809=DIRECTION('ref_axis',(1.,0.,0.));
#3810=DIRECTION('',(-1.23908819712629E-16,1.,0.));
#3811=DIRECTION('',(1.,0.,0.));
#3812=DIRECTION('',(0.,1.,0.));
#3813=DIRECTION('center_axis',(-1.,-1.23908819712629E-16,0.));
#3814=DIRECTION('ref_axis',(1.23908819712629E-16,-1.,0.));
#3815=DIRECTION('',(0.,0.,1.));
#3816=DIRECTION('',(0.,0.,-1.));
#3817=DIRECTION('center_axis',(-1.,-1.23908819712629E-16,0.));
#3818=DIRECTION('ref_axis',(1.23908819712629E-16,-1.,0.));
#3819=DIRECTION('',(0.,0.,1.));
#3820=DIRECTION('',(0.,0.,-1.));
#3821=DIRECTION('center_axis',(-1.,-1.23908819712629E-16,0.));
#3822=DIRECTION('ref_axis',(1.23908819712629E-16,-1.,0.));
#3823=DIRECTION('',(0.,0.,1.));
#3824=DIRECTION('',(0.,0.,-1.));
#3825=DIRECTION('center_axis',(-1.,-1.23908819712629E-16,0.));
#3826=DIRECTION('ref_axis',(1.23908819712629E-16,-1.,0.));
#3827=DIRECTION('',(0.,0.,1.));
#3828=DIRECTION('',(0.,0.,-1.));
#3829=DIRECTION('center_axis',(-1.,-1.23908819712629E-16,0.));
#3830=DIRECTION('ref_axis',(1.23908819712629E-16,-1.,0.));
#3831=DIRECTION('',(0.,0.,1.));
#3832=DIRECTION('',(0.,0.,-1.));
#3833=DIRECTION('center_axis',(-1.,-1.23908819712629E-16,0.));
#3834=DIRECTION('ref_axis',(1.23908819712629E-16,-1.,0.));
#3835=DIRECTION('',(0.,0.,1.));
#3836=DIRECTION('',(0.,0.,-1.));
#3837=DIRECTION('center_axis',(-1.,-1.23908819712629E-16,0.));
#3838=DIRECTION('ref_axis',(1.23908819712629E-16,-1.,0.));
#3839=DIRECTION('',(0.,0.,1.));
#3840=DIRECTION('',(0.,0.,-1.));
#3841=DIRECTION('center_axis',(-1.,-1.23908819712629E-16,0.));
#3842=DIRECTION('ref_axis',(1.23908819712629E-16,-1.,0.));
#3843=DIRECTION('',(0.,0.,1.));
#3844=DIRECTION('',(0.,0.,-1.));
#3845=DIRECTION('center_axis',(-1.,-1.23908819712629E-16,0.));
#3846=DIRECTION('ref_axis',(1.23908819712629E-16,-1.,0.));
#3847=DIRECTION('',(0.,0.,-1.));
#3848=DIRECTION('',(0.,0.,1.));
#3849=DIRECTION('center_axis',(-1.,0.,0.));
#3850=DIRECTION('ref_axis',(0.,0.,1.));
#3851=DIRECTION('',(0.,0.,-1.));
#3852=DIRECTION('',(0.,0.,-1.));
#3853=DIRECTION('',(0.,0.,1.));
#3854=DIRECTION('center_axis',(-0.766044443118972,-0.642787609686546,0.));
#3855=DIRECTION('ref_axis',(0.642787609686546,-0.766044443118972,0.));
#3856=DIRECTION('',(0.,0.,-1.));
#3857=DIRECTION('',(-0.642787609686546,0.766044443118972,0.));
#3858=DIRECTION('center_axis',(0.,-1.,0.));
#3859=DIRECTION('ref_axis',(0.,0.,-1.));
#3860=DIRECTION('',(0.,0.,-1.));
#3861=DIRECTION('',(0.,0.,-1.));
#3862=DIRECTION('center_axis',(0.96592582628907,-0.258819045102514,0.));
#3863=DIRECTION('ref_axis',(0.258819045102514,0.96592582628907,0.));
#3864=DIRECTION('',(0.,0.,-1.));
#3865=DIRECTION('center_axis',(0.766044443118972,0.642787609686546,0.));
#3866=DIRECTION('ref_axis',(-0.642787609686546,0.766044443118972,0.));
#3867=DIRECTION('',(0.,0.,1.));
#3868=DIRECTION('',(0.642787609686546,-0.766044443118972,0.));
#3869=DIRECTION('',(0.,0.,-1.));
#3870=DIRECTION('',(0.,0.,-1.));
#3871=DIRECTION('',(0.642787609686546,-0.766044443118972,0.));
#3872=DIRECTION('center_axis',(1.,-4.47692281884469E-17,0.));
#3873=DIRECTION('ref_axis',(4.47692281884469E-17,1.,0.));
#3874=DIRECTION('',(-4.47692281884469E-17,-1.,2.47817639425258E-17));
#3875=DIRECTION('',(0.,0.,1.));
#3876=DIRECTION('',(0.,0.,1.));
#3877=DIRECTION('',(0.,0.,1.));
#3878=DIRECTION('',(-4.47692281884469E-17,-1.,2.47817639425258E-17));
#3879=DIRECTION('',(0.,0.,-1.));
#3880=DIRECTION('center_axis',(0.,1.,0.));
#3881=DIRECTION('ref_axis',(0.,0.,1.));
#3882=DIRECTION('',(-1.,1.79745021839835E-17,5.55111512312578E-17));
#3883=DIRECTION('',(0.,0.,1.));
#3884=DIRECTION('',(0.,0.,-1.));
#3885=DIRECTION('center_axis',(-1.,-8.47613560090905E-17,0.));
#3886=DIRECTION('ref_axis',(8.47613560090905E-17,-1.,0.));
#3887=DIRECTION('',(0.,0.,-1.));
#3888=DIRECTION('',(1.79745021839835E-17,1.,-2.47817639425258E-17));
#3889=DIRECTION('',(5.55111512312578E-17,-9.97785309041681E-34,1.));
#3890=DIRECTION('',(1.79745021839835E-17,1.,-2.47817639425258E-17));
#3891=DIRECTION('',(0.,0.,-1.));
#3892=DIRECTION('',(0.,0.,1.));
#3893=DIRECTION('center_axis',(0.,1.,0.));
#3894=DIRECTION('ref_axis',(0.,0.,1.));
#3895=DIRECTION('center_axis',(-1.,-1.23908819712629E-16,0.));
#3896=DIRECTION('ref_axis',(1.23908819712629E-16,-1.,0.));
#3897=DIRECTION('',(0.,0.,-1.));
#3898=DIRECTION('center_axis',(0.,0.,1.));
#3899=DIRECTION('ref_axis',(-1.,1.22464679914735E-16,0.));
#3900=DIRECTION('center_axis',(0.,0.,1.));
#3901=DIRECTION('ref_axis',(-1.,1.22464679914735E-16,0.));
#3902=DIRECTION('center_axis',(0.,0.,1.));
#3903=DIRECTION('ref_axis',(-1.,1.22464679914735E-16,0.));
#3904=DIRECTION('center_axis',(0.,0.,1.));
#3905=DIRECTION('ref_axis',(-1.,1.22464679914735E-16,0.));
#3906=DIRECTION('center_axis',(0.,0.,1.));
#3907=DIRECTION('ref_axis',(-1.,1.22464679914735E-16,0.));
#3908=DIRECTION('center_axis',(0.,0.,1.));
#3909=DIRECTION('ref_axis',(-1.,1.22464679914735E-16,0.));
#3910=DIRECTION('center_axis',(0.,0.,1.));
#3911=DIRECTION('ref_axis',(-1.,1.22464679914735E-16,0.));
#3912=DIRECTION('center_axis',(0.,0.,1.));
#3913=DIRECTION('ref_axis',(-1.,1.22464679914735E-16,0.));
#3914=DIRECTION('center_axis',(0.,0.,1.));
#3915=DIRECTION('ref_axis',(-1.,1.22464679914735E-16,0.));
#3916=DIRECTION('center_axis',(0.342020143325676,-0.939692620785906,0.));
#3917=DIRECTION('ref_axis',(0.939692620785906,0.342020143325676,0.));
#3918=DIRECTION('',(0.939692620785906,0.342020143325676,0.));
#3919=DIRECTION('',(0.939692620785906,0.342020143325676,0.));
#3920=DIRECTION('center_axis',(-0.642787609686546,0.766044443118972,0.));
#3921=DIRECTION('ref_axis',(-0.766044443118972,-0.642787609686546,0.));
#3922=DIRECTION('',(-0.766044443118972,-0.642787609686546,0.));
#3923=DIRECTION('',(-0.766044443118972,-0.642787609686546,0.));
#3924=DIRECTION('center_axis',(0.,0.,1.));
#3925=DIRECTION('ref_axis',(1.,0.,0.));
#3926=DIRECTION('center_axis',(0.,0.,1.));
#3927=DIRECTION('ref_axis',(1.,0.,0.));
#3928=DIRECTION('center_axis',(5.55111512312578E-17,2.47817639425258E-17,
1.));
#3929=DIRECTION('ref_axis',(1.,0.,-5.55111512312578E-17));
#3930=DIRECTION('center_axis',(-5.55111512312578E-17,-2.47817639425258E-17,
-1.));
#3931=DIRECTION('ref_axis',(1.,-1.37566424599088E-33,-5.55111512312578E-17));
#3932=DIRECTION('center_axis',(-5.55111512312578E-17,-2.47817639425258E-17,
-1.));
#3933=DIRECTION('ref_axis',(1.,-1.37566424599088E-33,-5.55111512312578E-17));
#3934=DIRECTION('',(-1.,1.79745021839835E-17,5.55111512312578E-17));
#3935=DIRECTION('center_axis',(5.55111512312578E-17,2.47817639425258E-17,
1.));
#3936=DIRECTION('ref_axis',(1.,0.,-5.55111512312578E-17));
#3937=DIRECTION('center_axis',(5.55111512312578E-17,2.47817639425258E-17,
1.));
#3938=DIRECTION('ref_axis',(1.,-1.37566424599088E-33,-5.55111512312578E-17));
#3939=DIRECTION('',(-1.,1.79745021839835E-17,5.55111512312578E-17));
#3940=DIRECTION('center_axis',(5.55111512312578E-17,2.47817639425258E-17,
1.));
#3941=DIRECTION('ref_axis',(1.,-1.37566424599088E-33,-5.55111512312578E-17));
#3942=DIRECTION('center_axis',(-1.79745021839835E-17,-1.,0.));
#3943=DIRECTION('ref_axis',(1.,-1.79745021839835E-17,0.));
#3944=DIRECTION('center_axis',(0.,0.,-1.));
#3945=DIRECTION('ref_axis',(-1.,0.,0.));
#3946=DIRECTION('center_axis',(0.,0.,-1.));
#3947=DIRECTION('ref_axis',(-1.,0.,0.));
#3948=DIRECTION('center_axis',(0.,0.,-1.));
#3949=DIRECTION('ref_axis',(-1.,0.,0.));
#3950=DIRECTION('center_axis',(0.,0.,-1.));
#3951=DIRECTION('ref_axis',(-1.,0.,0.));
#3952=DIRECTION('axis',(0.,0.,1.));
#3953=DIRECTION('refdir',(1.,0.,0.));
#3954=DIRECTION('center_axis',(0.,0.,1.));
#3955=DIRECTION('ref_axis',(1.,0.,0.));
#3956=DIRECTION('center_axis',(0.,0.,1.));
#3957=DIRECTION('ref_axis',(1.,0.,0.));
#3958=DIRECTION('',(0.,0.,1.));
#3959=DIRECTION('center_axis',(-2.10053591606567E-33,2.47817639425258E-17,
-1.));
#3960=DIRECTION('ref_axis',(5.20549852247368E-50,1.,2.47817639425258E-17));
#3961=DIRECTION('center_axis',(0.,0.,1.));
#3962=DIRECTION('ref_axis',(1.,0.,0.));
#3963=DIRECTION('center_axis',(-2.10053591606567E-33,2.47817639425258E-17,
-1.));
#3964=DIRECTION('ref_axis',(5.20549852247368E-50,1.,2.47817639425258E-17));
#3965=DIRECTION('',(0.,0.,1.));
#3966=DIRECTION('center_axis',(0.,0.,1.));
#3967=DIRECTION('ref_axis',(1.,0.,0.));
#3968=DIRECTION('center_axis',(5.55111512312578E-17,0.,-1.));
#3969=DIRECTION('ref_axis',(-1.,0.,-5.55111512312578E-17));
#3970=DIRECTION('center_axis',(0.,0.,-1.));
#3971=DIRECTION('ref_axis',(-1.,0.,0.));
#3972=DIRECTION('',(5.55111512312578E-17,0.,-1.));
#3973=DIRECTION('center_axis',(0.,0.,1.));
#3974=DIRECTION('ref_axis',(1.,0.,0.));
#3975=DIRECTION('center_axis',(0.,0.,-1.));
#3976=DIRECTION('ref_axis',(-1.,0.,0.));
#3977=DIRECTION('',(1.34307684565341E-16,-1.,0.));
#3978=DIRECTION('center_axis',(0.,0.,1.));
#3979=DIRECTION('ref_axis',(-1.,0.,0.));
#3980=DIRECTION('',(1.,0.,0.));
#3981=DIRECTION('center_axis',(0.,0.,1.));
#3982=DIRECTION('ref_axis',(-1.,0.,0.));
#3983=DIRECTION('',(-8.47613560090905E-17,1.,0.));
#3984=DIRECTION('',(-0.939692620785907,-0.342020143325673,0.));
#3985=DIRECTION('center_axis',(0.,1.,0.));
#3986=DIRECTION('ref_axis',(0.,0.,1.));
#3987=DIRECTION('',(0.,0.,-1.));
#3988=DIRECTION('',(1.,8.47613560090905E-17,0.));
#3989=DIRECTION('',(0.,0.,1.));
#3990=DIRECTION('center_axis',(0.766044443118972,0.642787609686546,0.));
#3991=DIRECTION('ref_axis',(-0.642787609686546,0.766044443118972,0.));
#3992=DIRECTION('',(0.,0.,-1.));
#3993=DIRECTION('',(0.642787609686546,-0.766044443118972,0.));
#3994=DIRECTION('',(0.,0.,-1.));
#3995=DIRECTION('',(0.642787609686546,-0.766044443118972,0.));
#3996=DIRECTION('',(0.,0.,1.));
#3997=DIRECTION('',(-0.642787609686546,0.766044443118972,0.));
#3998=DIRECTION('',(0.,0.,-1.));
#3999=DIRECTION('',(-0.642787609686546,0.766044443118972,0.));
#4000=DIRECTION('center_axis',(0.,0.,-1.));
#4001=DIRECTION('ref_axis',(-1.,0.,0.));
#4002=DIRECTION('',(0.766044443118972,0.642787609686546,0.));
#4003=DIRECTION('',(0.,1.,0.));
#4004=DIRECTION('',(1.,0.,0.));
#4005=DIRECTION('',(-1.23908819712629E-16,1.,0.));
#4006=DIRECTION('center_axis',(0.,0.,1.));
#4007=DIRECTION('ref_axis',(1.,0.,0.));
#4008=DIRECTION('',(-1.23908819712629E-16,1.,0.));
#4009=DIRECTION('center_axis',(0.,0.,1.));
#4010=DIRECTION('ref_axis',(1.,0.,0.));
#4011=DIRECTION('',(-1.23908819712629E-16,1.,0.));
#4012=DIRECTION('center_axis',(0.,0.,1.));
#4013=DIRECTION('ref_axis',(1.,0.,0.));
#4014=DIRECTION('',(-1.23908819712629E-16,1.,0.));
#4015=DIRECTION('center_axis',(0.,0.,1.));
#4016=DIRECTION('ref_axis',(1.,0.,0.));
#4017=DIRECTION('',(-1.23908819712629E-16,1.,0.));
#4018=DIRECTION('center_axis',(0.,0.,1.));
#4019=DIRECTION('ref_axis',(1.,0.,0.));
#4020=DIRECTION('',(-1.23908819712629E-16,1.,0.));
#4021=DIRECTION('center_axis',(0.,0.,1.));
#4022=DIRECTION('ref_axis',(1.,0.,0.));
#4023=DIRECTION('',(-1.23908819712629E-16,1.,0.));
#4024=DIRECTION('center_axis',(0.,0.,1.));
#4025=DIRECTION('ref_axis',(1.,0.,0.));
#4026=DIRECTION('',(-1.23908819712629E-16,1.,0.));
#4027=DIRECTION('center_axis',(0.,0.,1.));
#4028=DIRECTION('ref_axis',(1.,0.,0.));
#4029=DIRECTION('',(-1.23908819712629E-16,1.,0.));
#4030=DIRECTION('center_axis',(0.,0.,1.));
#4031=DIRECTION('ref_axis',(1.,0.,0.));
#4032=DIRECTION('',(-1.23908819712629E-16,1.,0.));
#4033=DIRECTION('',(-1.,0.,0.));
#4034=DIRECTION('',(-0.258819045102514,-0.96592582628907,0.));
#4035=DIRECTION('center_axis',(0.,0.,-1.));
#4036=DIRECTION('ref_axis',(-1.,0.,0.));
#4037=DIRECTION('',(1.,0.,0.));
#4038=DIRECTION('center_axis',(0.,0.,-1.));
#4039=DIRECTION('ref_axis',(-1.,0.,0.));
#4040=DIRECTION('',(1.34307684565341E-16,-1.,0.));
#4041=DIRECTION('',(-0.939692620785907,-0.342020143325673,0.));
#4042=DIRECTION('',(-8.47613560090905E-17,1.,0.));
#4043=DIRECTION('center_axis',(0.,0.,-1.));
#4044=DIRECTION('ref_axis',(-1.,0.,0.));
#4045=DIRECTION('center_axis',(-0.766044443118972,-0.642787609686546,0.));
#4046=DIRECTION('ref_axis',(0.642787609686546,-0.766044443118972,0.));
#4047=DIRECTION('',(0.,0.,-1.));
#4048=DIRECTION('',(0.642787609686547,-0.766044443118972,0.));
#4049=DIRECTION('',(0.,0.,-1.));
#4050=DIRECTION('',(0.642787609686547,-0.766044443118972,0.));
#4051=DIRECTION('center_axis',(0.,0.,-1.));
#4052=DIRECTION('ref_axis',(-1.,0.,0.));
#4053=DIRECTION('',(0.766044443118972,0.642787609686546,0.));
#4054=DIRECTION('',(-0.258819045102514,-0.96592582628907,0.));
#4055=DIRECTION('',(-1.,0.,0.));
#4056=DIRECTION('',(-1.23908819712629E-16,1.,0.));
#4057=DIRECTION('center_axis',(0.,0.,1.));
#4058=DIRECTION('ref_axis',(1.,0.,0.));
#4059=DIRECTION('',(-1.23908819712629E-16,1.,0.));
#4060=DIRECTION('center_axis',(0.,0.,1.));
#4061=DIRECTION('ref_axis',(1.,0.,0.));
#4062=DIRECTION('',(-1.23908819712629E-16,1.,0.));
#4063=DIRECTION('center_axis',(0.,0.,1.));
#4064=DIRECTION('ref_axis',(1.,0.,0.));
#4065=DIRECTION('',(-1.23908819712629E-16,1.,0.));
#4066=DIRECTION('center_axis',(0.,0.,1.));
#4067=DIRECTION('ref_axis',(1.,0.,0.));
#4068=DIRECTION('',(-1.23908819712629E-16,1.,0.));
#4069=DIRECTION('center_axis',(0.,0.,1.));
#4070=DIRECTION('ref_axis',(1.,0.,0.));
#4071=DIRECTION('',(-1.23908819712629E-16,1.,0.));
#4072=DIRECTION('center_axis',(0.,0.,1.));
#4073=DIRECTION('ref_axis',(1.,0.,0.));
#4074=DIRECTION('',(-1.23908819712629E-16,1.,0.));
#4075=DIRECTION('center_axis',(0.,0.,1.));
#4076=DIRECTION('ref_axis',(1.,0.,0.));
#4077=DIRECTION('',(-1.23908819712629E-16,1.,0.));
#4078=DIRECTION('center_axis',(0.,0.,1.));
#4079=DIRECTION('ref_axis',(1.,0.,0.));
#4080=DIRECTION('',(-1.23908819712629E-16,1.,0.));
#4081=DIRECTION('center_axis',(0.,0.,1.));
#4082=DIRECTION('ref_axis',(1.,0.,0.));
#4083=DIRECTION('',(-1.23908819712629E-16,1.,0.));
#4084=DIRECTION('',(1.,0.,0.));
#4085=DIRECTION('',(0.,1.,0.));
#4086=DIRECTION('center_axis',(-1.,-1.23908819712629E-16,0.));
#4087=DIRECTION('ref_axis',(1.23908819712629E-16,-1.,0.));
#4088=DIRECTION('',(0.,0.,1.));
#4089=DIRECTION('',(0.,0.,-1.));
#4090=DIRECTION('center_axis',(-1.,-1.23908819712629E-16,0.));
#4091=DIRECTION('ref_axis',(1.23908819712629E-16,-1.,0.));
#4092=DIRECTION('',(0.,0.,1.));
#4093=DIRECTION('',(0.,0.,-1.));
#4094=DIRECTION('center_axis',(-1.,-1.23908819712629E-16,0.));
#4095=DIRECTION('ref_axis',(1.23908819712629E-16,-1.,0.));
#4096=DIRECTION('',(0.,0.,1.));
#4097=DIRECTION('',(0.,0.,-1.));
#4098=DIRECTION('center_axis',(-1.,-1.23908819712629E-16,0.));
#4099=DIRECTION('ref_axis',(1.23908819712629E-16,-1.,0.));
#4100=DIRECTION('',(0.,0.,1.));
#4101=DIRECTION('',(0.,0.,-1.));
#4102=DIRECTION('center_axis',(-1.,-1.23908819712629E-16,0.));
#4103=DIRECTION('ref_axis',(1.23908819712629E-16,-1.,0.));
#4104=DIRECTION('',(0.,0.,1.));
#4105=DIRECTION('',(0.,0.,-1.));
#4106=DIRECTION('center_axis',(-1.,-1.23908819712629E-16,0.));
#4107=DIRECTION('ref_axis',(1.23908819712629E-16,-1.,0.));
#4108=DIRECTION('',(0.,0.,1.));
#4109=DIRECTION('',(0.,0.,-1.));
#4110=DIRECTION('center_axis',(-1.,-1.23908819712629E-16,0.));
#4111=DIRECTION('ref_axis',(1.23908819712629E-16,-1.,0.));
#4112=DIRECTION('',(0.,0.,1.));
#4113=DIRECTION('',(0.,0.,-1.));
#4114=DIRECTION('center_axis',(-1.,-1.23908819712629E-16,0.));
#4115=DIRECTION('ref_axis',(1.23908819712629E-16,-1.,0.));
#4116=DIRECTION('',(0.,0.,1.));
#4117=DIRECTION('',(0.,0.,-1.));
#4118=DIRECTION('center_axis',(-1.,-1.23908819712629E-16,0.));
#4119=DIRECTION('ref_axis',(1.23908819712629E-16,-1.,0.));
#4120=DIRECTION('',(0.,0.,-1.));
#4121=DIRECTION('',(0.,0.,1.));
#4122=DIRECTION('center_axis',(-1.,0.,0.));
#4123=DIRECTION('ref_axis',(0.,0.,1.));
#4124=DIRECTION('',(0.,0.,-1.));
#4125=DIRECTION('',(0.,0.,-1.));
#4126=DIRECTION('',(0.,0.,1.));
#4127=DIRECTION('center_axis',(0.,-1.,0.));
#4128=DIRECTION('ref_axis',(0.,0.,-1.));
#4129=DIRECTION('',(0.,0.,-1.));
#4130=DIRECTION('',(0.,0.,-1.));
#4131=DIRECTION('center_axis',(0.96592582628907,-0.258819045102514,0.));
#4132=DIRECTION('ref_axis',(0.258819045102514,0.96592582628907,0.));
#4133=DIRECTION('center_axis',(1.,1.34307684565341E-16,0.));
#4134=DIRECTION('ref_axis',(-1.34307684565341E-16,1.,0.));
#4135=DIRECTION('',(0.,0.,1.));
#4136=DIRECTION('',(-1.34307684565341E-16,1.,2.47817639425258E-17));
#4137=DIRECTION('',(0.,0.,-1.));
#4138=DIRECTION('',(-1.34307684565341E-16,1.,2.47817639425258E-17));
#4139=DIRECTION('',(0.,0.,1.));
#4140=DIRECTION('',(0.,0.,-1.));
#4141=DIRECTION('',(0.,0.,1.));
#4142=DIRECTION('center_axis',(0.,1.,0.));
#4143=DIRECTION('ref_axis',(0.,0.,1.));
#4144=DIRECTION('',(1.,8.47613560090905E-17,0.));
#4145=DIRECTION('',(0.,0.,-1.));
#4146=DIRECTION('',(0.,0.,1.));
#4147=DIRECTION('center_axis',(-1.,-8.47613560090905E-17,0.));
#4148=DIRECTION('ref_axis',(8.47613560090905E-17,-1.,0.));
#4149=DIRECTION('',(0.,0.,-1.));
#4150=DIRECTION('',(-8.47613560090905E-17,1.,2.47817639425258E-17));
#4151=DIRECTION('',(0.,0.,-1.));
#4152=DIRECTION('',(-8.47613560090905E-17,1.,2.47817639425258E-17));
#4153=DIRECTION('',(0.,0.,-1.));
#4154=DIRECTION('',(0.,0.,1.));
#4155=DIRECTION('',(0.,0.,-1.));
#4156=DIRECTION('center_axis',(0.,1.,0.));
#4157=DIRECTION('ref_axis',(0.,0.,1.));
#4158=DIRECTION('center_axis',(-1.,-1.23908819712629E-16,0.));
#4159=DIRECTION('ref_axis',(1.23908819712629E-16,-1.,0.));
#4160=DIRECTION('',(0.,0.,-1.));
#4161=DIRECTION('center_axis',(0.,0.,1.));
#4162=DIRECTION('ref_axis',(-1.,1.22464679914735E-16,0.));
#4163=DIRECTION('center_axis',(0.,0.,1.));
#4164=DIRECTION('ref_axis',(-1.,1.22464679914735E-16,0.));
#4165=DIRECTION('center_axis',(0.,0.,1.));
#4166=DIRECTION('ref_axis',(-1.,1.22464679914735E-16,0.));
#4167=DIRECTION('center_axis',(0.,0.,1.));
#4168=DIRECTION('ref_axis',(-1.,1.22464679914735E-16,0.));
#4169=DIRECTION('center_axis',(0.,0.,1.));
#4170=DIRECTION('ref_axis',(-1.,1.22464679914735E-16,0.));
#4171=DIRECTION('center_axis',(0.,0.,1.));
#4172=DIRECTION('ref_axis',(-1.,1.22464679914735E-16,0.));
#4173=DIRECTION('center_axis',(0.,0.,1.));
#4174=DIRECTION('ref_axis',(-1.,1.22464679914735E-16,0.));
#4175=DIRECTION('center_axis',(0.,0.,1.));
#4176=DIRECTION('ref_axis',(-1.,1.22464679914735E-16,0.));
#4177=DIRECTION('center_axis',(0.,0.,1.));
#4178=DIRECTION('ref_axis',(-1.,1.22464679914735E-16,0.));
#4179=DIRECTION('center_axis',(-0.342020143325673,0.939692620785907,0.));
#4180=DIRECTION('ref_axis',(-0.939692620785907,-0.342020143325673,0.));
#4181=DIRECTION('',(-0.939692620785907,-0.342020143325673,0.));
#4182=DIRECTION('center_axis',(0.642787609686546,-0.766044443118972,0.));
#4183=DIRECTION('ref_axis',(0.766044443118972,0.642787609686546,0.));
#4184=DIRECTION('',(0.766044443118972,0.642787609686546,0.));
#4185=DIRECTION('center_axis',(0.,0.,1.));
#4186=DIRECTION('ref_axis',(1.,0.,0.));
#4187=DIRECTION('center_axis',(-0.342020143325673,0.939692620785907,0.));
#4188=DIRECTION('ref_axis',(-0.939692620785907,-0.342020143325673,0.));
#4189=DIRECTION('',(-0.939692620785907,-0.342020143325673,0.));
#4190=DIRECTION('center_axis',(0.642787609686546,-0.766044443118972,0.));
#4191=DIRECTION('ref_axis',(0.766044443118972,0.642787609686546,0.));
#4192=DIRECTION('',(0.766044443118972,0.642787609686546,0.));
#4193=DIRECTION('center_axis',(0.,0.,-1.));
#4194=DIRECTION('ref_axis',(1.,0.,0.));
#4195=DIRECTION('center_axis',(-2.10053591606567E-33,2.47817639425258E-17,
-1.));
#4196=DIRECTION('ref_axis',(0.,1.,2.47817639425258E-17));
#4197=DIRECTION('center_axis',(2.10053591606567E-33,-2.47817639425258E-17,
1.));
#4198=DIRECTION('ref_axis',(5.20549852247368E-50,1.,2.47817639425258E-17));
#4199=DIRECTION('center_axis',(2.10053591606567E-33,-2.47817639425258E-17,
1.));
#4200=DIRECTION('ref_axis',(5.20549852247368E-50,1.,2.47817639425258E-17));
#4201=DIRECTION('',(1.,8.47613560090905E-17,0.));
#4202=DIRECTION('center_axis',(-2.10053591606567E-33,2.47817639425258E-17,
-1.));
#4203=DIRECTION('ref_axis',(0.,1.,2.47817639425258E-17));
#4204=DIRECTION('center_axis',(-2.10053591606567E-33,2.47817639425258E-17,
-1.));
#4205=DIRECTION('ref_axis',(5.20549852247368E-50,1.,2.47817639425258E-17));
#4206=DIRECTION('',(1.,8.47613560090905E-17,0.));
#4207=DIRECTION('center_axis',(-2.10053591606567E-33,2.47817639425258E-17,
-1.));
#4208=DIRECTION('ref_axis',(5.20549852247368E-50,1.,2.47817639425258E-17));
#4209=DIRECTION('center_axis',(8.47613560090905E-17,-1.,0.));
#4210=DIRECTION('ref_axis',(1.,8.47613560090905E-17,0.));
#4211=DIRECTION('center_axis',(0.,0.,-1.));
#4212=DIRECTION('ref_axis',(-1.,0.,0.));
#4213=DIRECTION('center_axis',(0.,0.,-1.));
#4214=DIRECTION('ref_axis',(-1.,0.,0.));
#4215=DIRECTION('center_axis',(0.,0.,-1.));
#4216=DIRECTION('ref_axis',(-1.,0.,0.));
#4217=DIRECTION('center_axis',(0.,0.,-1.));
#4218=DIRECTION('ref_axis',(-1.,0.,0.));
#4219=DIRECTION('axis',(0.,0.,1.));
#4220=DIRECTION('refdir',(1.,0.,0.));
#4221=DIRECTION('center_axis',(0.,0.,-1.));
#4222=DIRECTION('ref_axis',(-1.,0.,0.));
#4223=DIRECTION('center_axis',(0.,0.,-1.));
#4224=DIRECTION('ref_axis',(-1.,0.,0.));
#4225=DIRECTION('',(0.,0.,-1.));
#4226=DIRECTION('center_axis',(0.,0.,-1.));
#4227=DIRECTION('ref_axis',(-1.,0.,0.));
#4228=DIRECTION('center_axis',(1.,0.,0.));
#4229=DIRECTION('ref_axis',(0.,0.,-1.));
#4230=DIRECTION('',(0.,1.,0.));
#4231=DIRECTION('',(0.,0.,1.));
#4232=DIRECTION('',(0.,1.,0.));
#4233=DIRECTION('center_axis',(1.,0.,0.));
#4234=DIRECTION('ref_axis',(0.,0.,-1.));
#4235=DIRECTION('',(0.,1.,0.));
#4236=DIRECTION('',(0.,0.,-1.));
#4237=DIRECTION('',(0.,1.,0.));
#4238=DIRECTION('',(0.,0.948683298050515,0.316227766016835));
#4239=DIRECTION('',(0.,-0.948683298050515,0.316227766016835));
#4240=DIRECTION('center_axis',(0.,0.,-1.));
#4241=DIRECTION('ref_axis',(-1.,0.,0.));
#4242=DIRECTION('center_axis',(0.,0.,-1.));
#4243=DIRECTION('ref_axis',(-1.,0.,0.));
#4244=DIRECTION('',(0.,1.,0.));
#4245=DIRECTION('center_axis',(0.,0.,-1.));
#4246=DIRECTION('ref_axis',(-1.,0.,0.));
#4247=DIRECTION('center_axis',(0.,0.,-1.));
#4248=DIRECTION('ref_axis',(-1.,0.,0.));
#4249=DIRECTION('center_axis',(0.,0.,1.));
#4250=DIRECTION('ref_axis',(-1.,0.,0.));
#4251=DIRECTION('center_axis',(0.,0.,1.));
#4252=DIRECTION('ref_axis',(-1.,0.,0.));
#4253=DIRECTION('',(0.,-1.,0.));
#4254=DIRECTION('center_axis',(0.,0.,-1.));
#4255=DIRECTION('ref_axis',(-1.,0.,0.));
#4256=DIRECTION('center_axis',(0.,0.,-1.));
#4257=DIRECTION('ref_axis',(-1.,0.,0.));
#4258=DIRECTION('',(0.948683298050515,0.,0.316227766016835));
#4259=DIRECTION('center_axis',(-0.316227766016835,0.,0.948683298050515));
#4260=DIRECTION('ref_axis',(0.,-1.,0.));
#4261=DIRECTION('',(0.948683298050515,0.,0.316227766016835));
#4262=DIRECTION('',(0.,1.,0.));
#4263=DIRECTION('center_axis',(0.,0.,1.));
#4264=DIRECTION('ref_axis',(1.,0.,0.));
#4265=DIRECTION('',(-0.948683298050515,0.,0.316227766016835));
#4266=DIRECTION('center_axis',(0.,0.,-1.));
#4267=DIRECTION('ref_axis',(-1.,0.,0.));
#4268=DIRECTION('center_axis',(0.,0.,-1.));
#4269=DIRECTION('ref_axis',(-1.,0.,0.));
#4270=DIRECTION('center_axis',(0.316227766016835,0.,0.948683298050515));
#4271=DIRECTION('ref_axis',(0.,-1.,0.));
#4272=DIRECTION('',(-0.948683298050515,0.,0.316227766016835));
#4273=DIRECTION('center_axis',(0.,0.,1.));
#4274=DIRECTION('ref_axis',(1.,0.,0.));
#4275=DIRECTION('center_axis',(0.,0.,1.));
#4276=DIRECTION('ref_axis',(1.,0.,0.));
#4277=DIRECTION('axis',(0.,0.,1.));
#4278=DIRECTION('refdir',(1.,0.,0.));
#4279=DIRECTION('center_axis',(4.4406667760173E-16,2.77555573237168E-17,
1.));
#4280=DIRECTION('ref_axis',(1.,-2.43623723452952E-32,-4.4406667760173E-16));
#4281=DIRECTION('center_axis',(4.4406667760173E-16,2.77555573237168E-17,
1.));
#4282=DIRECTION('ref_axis',(1.,-2.43623723452952E-32,-4.4406667760173E-16));
#4283=DIRECTION('',(4.4406667760173E-16,2.77555573237168E-17,1.));
#4284=DIRECTION('center_axis',(-4.4406667760173E-16,-2.77555573237168E-17,
-1.));
#4285=DIRECTION('ref_axis',(-1.,2.46506362514545E-32,4.4406667760173E-16));
#4286=DIRECTION('center_axis',(4.4406667760173E-16,2.77555573237168E-17,
1.));
#4287=DIRECTION('ref_axis',(1.,-2.43623723453099E-32,-4.4406667760173E-16));
#4288=DIRECTION('center_axis',(4.4406667760173E-16,2.77555573237168E-17,
1.));
#4289=DIRECTION('ref_axis',(1.,-2.436237234531E-32,-4.4406667760173E-16));
#4290=DIRECTION('center_axis',(-0.316227766016829,3.0018299425529E-15,-0.948683298050517));
#4291=DIRECTION('ref_axis',(0.948683298050517,-9.96757165847559E-13,-0.316227766016829));
#4292=DIRECTION('center_axis',(-0.316227766016834,-7.50457485638231E-16,
0.948683298050515));
#4293=DIRECTION('ref_axis',(0.948683298050515,-6.16711447781422E-12,0.316227766016834));
#4294=DIRECTION('center_axis',(4.4406667760173E-16,2.77555573237168E-17,
1.));
#4295=DIRECTION('ref_axis',(1.,-2.436237234531E-32,-4.4406667760173E-16));
#4296=DIRECTION('center_axis',(-0.316227766016829,3.11728494034299E-15,
-0.948683298050517));
#4297=DIRECTION('ref_axis',(0.948683298050517,1.56058638540273E-11,-0.316227766016829));
#4298=DIRECTION('center_axis',(-0.316227766016834,-7.50457485638232E-16,
0.948683298050515));
#4299=DIRECTION('ref_axis',(0.948683298050515,-6.59186276791152E-12,0.316227766016834));
#4300=DIRECTION('center_axis',(4.4406667760173E-16,2.77555573237168E-17,
1.));
#4301=DIRECTION('ref_axis',(1.,-2.436237234531E-32,-4.4406667760173E-16));
#4302=DIRECTION('center_axis',(-0.31622776601683,2.77091994697168E-15,-0.948683298050517));
#4303=DIRECTION('ref_axis',(0.948683298050517,2.37176708321596E-12,-0.31622776601683));
#4304=DIRECTION('center_axis',(-0.316227766016833,3.4636499337146E-16,0.948683298050515));
#4305=DIRECTION('ref_axis',(0.948683298050515,3.44351511508786E-12,0.316227766016833));
#4306=DIRECTION('center_axis',(4.4406667760173E-16,2.77555573237168E-17,
1.));
#4307=DIRECTION('ref_axis',(1.,-2.436237234531E-32,-4.4406667760173E-16));
#4308=DIRECTION('center_axis',(-0.31622776601683,2.77091994697168E-15,-0.948683298050517));
#4309=DIRECTION('ref_axis',(0.948683298050517,-7.95145482367482E-13,-0.31622776601683));
#4310=DIRECTION('center_axis',(-0.316227766016833,3.4636499337146E-16,0.948683298050515));
#4311=DIRECTION('ref_axis',(0.948683298050515,-1.06976938896506E-12,0.316227766016833));
#4312=DIRECTION('center_axis',(4.4406667760173E-16,2.77555573237168E-17,
1.));
#4313=DIRECTION('ref_axis',(1.,-2.436237234531E-32,-4.4406667760173E-16));
#4314=DIRECTION('center_axis',(-0.316227766016832,-2.02046246133356E-16,
-0.948683298050516));
#4315=DIRECTION('ref_axis',(0.948683298050516,2.39882550987045E-12,-0.316227766016832));
#4316=DIRECTION('center_axis',(-0.316227766016834,1.15454997790497E-16,
0.948683298050515));
#4317=DIRECTION('ref_axis',(0.948683298050515,4.35170492897026E-12,0.316227766016834));
#4318=DIRECTION('center_axis',(4.4406667760173E-16,2.77555573237168E-17,
1.));
#4319=DIRECTION('ref_axis',(1.,-2.43623723452951E-32,-4.4406667760173E-16));
#4320=DIRECTION('center_axis',(4.4406667760173E-16,2.77555573237168E-17,
1.));
#4321=DIRECTION('ref_axis',(1.,-2.43623723452951E-32,-4.4406667760173E-16));
#4322=DIRECTION('center_axis',(4.4406667760173E-16,2.77555573237168E-17,
1.));
#4323=DIRECTION('ref_axis',(1.,-2.43623723453053E-32,-4.4406667760173E-16));
#4324=DIRECTION('center_axis',(1.,6.93889390390723E-17,-4.4406667760173E-16));
#4325=DIRECTION('ref_axis',(-4.4406667760173E-16,-2.77555573237168E-17,
-1.));
#4326=DIRECTION('',(6.93889390390723E-17,1.,2.77555573237168E-17));
#4327=DIRECTION('',(4.4406667760173E-16,2.77555573237168E-17,1.));
#4328=DIRECTION('',(6.93889390390723E-17,1.,2.77555573237168E-17));
#4329=DIRECTION('center_axis',(1.,6.93889390390723E-17,-4.4406667760173E-16));
#4330=DIRECTION('ref_axis',(-4.4406667760173E-16,-2.77555573237168E-17,
-1.));
#4331=DIRECTION('',(6.93889390390723E-17,1.,2.77555573237168E-17));
#4332=DIRECTION('',(-4.4406667760173E-16,-2.77555573237168E-17,-1.));
#4333=DIRECTION('',(6.93889390390723E-17,1.,2.77555573237168E-17));
#4334=DIRECTION('',(2.06254340956326E-16,0.948683298050515,0.316227766016835));
#4335=DIRECTION('',(-4.4406667760173E-16,-2.77555573237168E-17,-1.));
#4336=DIRECTION('',(7.45980858847001E-17,-0.948683298050515,0.316227766016835));
#4337=DIRECTION('center_axis',(4.4406667760173E-16,-2.77555573237167E-17,
-1.));
#4338=DIRECTION('ref_axis',(-1.,-6.93889390390723E-17,-4.4406667760173E-16));
#4339=DIRECTION('center_axis',(-4.4406667760173E-16,-2.77555573237168E-17,
-1.));
#4340=DIRECTION('ref_axis',(-1.,2.60819515195191E-32,4.4406667760173E-16));
#4341=DIRECTION('',(6.93889390390723E-17,1.,2.77555573237168E-17));
#4342=DIRECTION('center_axis',(-4.4406667760173E-16,-2.77555573237168E-17,
-1.));
#4343=DIRECTION('ref_axis',(-1.,2.43623723452952E-32,4.4406667760173E-16));
#4344=DIRECTION('center_axis',(4.4406667760173E-16,-2.77555573237167E-17,
-1.));
#4345=DIRECTION('ref_axis',(-1.,-6.93889390390723E-17,-4.4406667760173E-16));
#4346=DIRECTION('center_axis',(4.4406667760173E-16,2.77555573237168E-17,
1.));
#4347=DIRECTION('ref_axis',(-1.,2.46506362514546E-32,4.4406667760173E-16));
#4348=DIRECTION('center_axis',(4.4406667760173E-16,2.77555573237168E-17,
1.));
#4349=DIRECTION('ref_axis',(-1.,2.46506362514546E-32,4.4406667760173E-16));
#4350=DIRECTION('',(-6.93889390390723E-17,-1.,-2.77555573237168E-17));
#4351=DIRECTION('center_axis',(-4.4406667760173E-16,-2.77555573237168E-17,
-1.));
#4352=DIRECTION('ref_axis',(-1.,2.46506362514546E-32,4.4406667760173E-16));
#4353=DIRECTION('center_axis',(-4.4406667760173E-16,-2.77555573237168E-17,
-1.));
#4354=DIRECTION('ref_axis',(-1.,2.43623723452952E-32,4.4406667760173E-16));
#4355=DIRECTION('',(0.948683298050515,7.46052054228444E-17,0.316227766016835));
#4356=DIRECTION('center_axis',(-4.4406667760173E-16,-2.77555573237168E-17,
-1.));
#4357=DIRECTION('ref_axis',(-1.,2.43623723452952E-32,4.4406667760173E-16));
#4358=DIRECTION('center_axis',(-0.316227766016835,-4.38852448248957E-18,
0.948683298050515));
#4359=DIRECTION('ref_axis',(-6.93889390390723E-17,-1.,-2.77555573237168E-17));
#4360=DIRECTION('',(6.93889390390723E-17,1.,2.77555573237168E-17));
#4361=DIRECTION('',(0.948683298050515,7.46052054228444E-17,0.316227766016835));
#4362=DIRECTION('',(6.93889390390723E-17,1.,2.77555573237168E-17));
#4363=DIRECTION('',(6.93889390390723E-17,1.,2.77555573237168E-17));
#4364=DIRECTION('',(6.93889390390723E-17,1.,2.77555573237168E-17));
#4365=DIRECTION('',(6.93889390390723E-17,1.,2.77555573237168E-17));
#4366=DIRECTION('center_axis',(4.4406667760173E-16,2.77555573237168E-17,
1.));
#4367=DIRECTION('ref_axis',(1.,-2.43623723452952E-32,-4.4406667760173E-16));
#4368=DIRECTION('',(-0.948683298050515,-5.7051049648782E-17,0.316227766016835));
#4369=DIRECTION('center_axis',(-4.4406667760173E-16,-2.77555573237168E-17,
-1.));
#4370=DIRECTION('ref_axis',(-1.,2.46506362514546E-32,4.4406667760173E-16));
#4371=DIRECTION('center_axis',(-4.4406667760173E-16,-2.77555573237168E-17,
-1.));
#4372=DIRECTION('ref_axis',(-1.,2.43623723452952E-32,4.4406667760173E-16));
#4373=DIRECTION('center_axis',(-4.4406667760173E-16,-2.77555573237168E-17,
-1.));
#4374=DIRECTION('ref_axis',(-1.,2.43623723452952E-32,4.4406667760173E-16));
#4375=DIRECTION('center_axis',(-4.4406667760173E-16,-2.77555573237168E-17,
-1.));
#4376=DIRECTION('ref_axis',(-1.,2.43623723452952E-32,4.4406667760173E-16));
#4377=DIRECTION('center_axis',(-4.4406667760173E-16,-2.77555573237168E-17,
-1.));
#4378=DIRECTION('ref_axis',(-1.,2.43623723452952E-32,4.4406667760173E-16));
#4379=DIRECTION('center_axis',(0.316227766016835,-4.8273942839698E-17,0.948683298050515));
#4380=DIRECTION('ref_axis',(-6.93889390390723E-17,-1.,-2.77555573237168E-17));
#4381=DIRECTION('',(-0.948683298050515,-5.7051049648782E-17,0.316227766016835));
#4382=DIRECTION('center_axis',(4.4406667760173E-16,2.77555573237168E-17,
1.));
#4383=DIRECTION('ref_axis',(1.,-2.43623723452952E-32,-4.4406667760173E-16));
#4384=DIRECTION('center_axis',(4.4406667760173E-16,2.77555573237168E-17,
1.));
#4385=DIRECTION('ref_axis',(1.,-2.43623723452951E-32,-4.4406667760173E-16));
#4386=DIRECTION('center_axis',(4.4406667760173E-16,2.77555573237168E-17,
1.));
#4387=DIRECTION('ref_axis',(1.,-2.60819515195191E-32,-4.4406667760173E-16));
#4388=DIRECTION('axis',(0.,0.,1.));
#4389=DIRECTION('refdir',(1.,0.,0.));
#4390=DIRECTION('center_axis',(0.,0.,-1.));
#4391=DIRECTION('ref_axis',(-1.,0.,0.));
#4392=DIRECTION('center_axis',(0.,0.,-1.));
#4393=DIRECTION('ref_axis',(-1.,0.,0.));
#4394=DIRECTION('',(0.,0.,-1.));
#4395=DIRECTION('center_axis',(0.,0.,-1.));
#4396=DIRECTION('ref_axis',(-1.,0.,0.));
#4397=DIRECTION('center_axis',(0.,-1.,0.));
#4398=DIRECTION('ref_axis',(0.,0.,-1.));
#4399=DIRECTION('center_axis',(0.,1.,0.));
#4400=DIRECTION('ref_axis',(0.,0.,1.));
#4401=DIRECTION('center_axis',(0.,1.,0.));
#4402=DIRECTION('ref_axis',(0.,0.,1.));
#4403=DIRECTION('center_axis',(0.,1.,0.));
#4404=DIRECTION('ref_axis',(0.,0.,1.));
#4405=DIRECTION('',(0.,1.,0.));
#4406=DIRECTION('center_axis',(0.,1.,0.));
#4407=DIRECTION('ref_axis',(0.,0.,1.));
#4408=DIRECTION('center_axis',(0.,1.,0.));
#4409=DIRECTION('ref_axis',(0.,0.,1.));
#4410=DIRECTION('center_axis',(0.,1.,0.));
#4411=DIRECTION('ref_axis',(0.,0.,1.));
#4412=DIRECTION('center_axis',(0.,1.,0.));
#4413=DIRECTION('ref_axis',(0.,0.,1.));
#4414=DIRECTION('center_axis',(0.,1.,0.));
#4415=DIRECTION('ref_axis',(0.,0.,1.));
#4416=DIRECTION('center_axis',(0.,1.,0.));
#4417=DIRECTION('ref_axis',(0.,0.,1.));
#4418=DIRECTION('center_axis',(0.,1.,0.));
#4419=DIRECTION('ref_axis',(0.,0.,1.));
#4420=DIRECTION('center_axis',(0.,1.,0.));
#4421=DIRECTION('ref_axis',(0.,0.,1.));
#4422=DIRECTION('center_axis',(0.,1.,0.));
#4423=DIRECTION('ref_axis',(0.,0.,1.));
#4424=DIRECTION('center_axis',(0.,-1.,0.));
#4425=DIRECTION('ref_axis',(0.,0.,-1.));
#4426=DIRECTION('',(1.,0.,0.));
#4427=DIRECTION('',(0.,0.,1.));
#4428=DIRECTION('center_axis',(0.,-1.,0.));
#4429=DIRECTION('ref_axis',(0.,0.,-1.));
#4430=DIRECTION('',(1.,0.,0.));
#4431=DIRECTION('',(0.,0.,-1.));
#4432=DIRECTION('center_axis',(0.,-1.,0.));
#4433=DIRECTION('ref_axis',(0.,0.,-1.));
#4434=DIRECTION('',(0.,0.,-1.));
#4435=DIRECTION('',(1.,0.,0.));
#4436=DIRECTION('center_axis',(1.,0.,0.));
#4437=DIRECTION('ref_axis',(0.,0.,-1.));
#4438=DIRECTION('',(0.,1.,0.));
#4439=DIRECTION('',(0.,0.,-1.));
#4440=DIRECTION('',(0.,1.,0.));
#4441=DIRECTION('',(0.,0.,1.));
#4442=DIRECTION('',(0.,0.,1.));
#4443=DIRECTION('center_axis',(1.,0.,0.));
#4444=DIRECTION('ref_axis',(0.,0.,-1.));
#4445=DIRECTION('',(0.,1.,0.));
#4446=DIRECTION('',(0.,0.,1.));
#4447=DIRECTION('',(0.,1.,0.));
#4448=DIRECTION('',(0.,0.,-1.));
#4449=DIRECTION('',(0.,0.,-1.));
#4450=DIRECTION('center_axis',(0.,-1.,0.));
#4451=DIRECTION('ref_axis',(0.,0.,-1.));
#4452=DIRECTION('',(0.,0.,1.));
#4453=DIRECTION('',(1.,0.,0.));
#4454=DIRECTION('center_axis',(0.,0.,-1.));
#4455=DIRECTION('ref_axis',(-1.,0.,0.));
#4456=DIRECTION('center_axis',(0.,0.,-1.));
#4457=DIRECTION('ref_axis',(-1.,0.,0.));
#4458=DIRECTION('center_axis',(0.,0.,-1.));
#4459=DIRECTION('ref_axis',(-1.,0.,0.));
#4460=DIRECTION('center_axis',(0.,0.,-1.));
#4461=DIRECTION('ref_axis',(-1.,0.,0.));
#4462=DIRECTION('center_axis',(0.,0.,-1.));
#4463=DIRECTION('ref_axis',(-1.,0.,0.));
#4464=DIRECTION('center_axis',(0.,0.,1.));
#4465=DIRECTION('ref_axis',(-1.,0.,0.));
#4466=DIRECTION('center_axis',(0.,0.,1.));
#4467=DIRECTION('ref_axis',(-1.,0.,0.));
#4468=DIRECTION('center_axis',(0.,0.,1.));
#4469=DIRECTION('ref_axis',(-1.,0.,0.));
#4470=DIRECTION('center_axis',(0.866025403784439,0.,0.5));
#4471=DIRECTION('ref_axis',(0.5,0.,-0.866025403784439));
#4472=DIRECTION('',(0.499999999999999,0.,-0.866025403784439));
#4473=DIRECTION('',(0.499999999999999,0.,-0.866025403784439));
#4474=DIRECTION('',(0.,1.,0.));
#4475=DIRECTION('',(0.5,0.,-0.866025403784439));
#4476=DIRECTION('',(0.,1.,0.));
#4477=DIRECTION('center_axis',(2.46473488855316E-16,0.,1.));
#4478=DIRECTION('ref_axis',(1.,0.,-2.46473488855316E-16));
#4479=DIRECTION('',(1.,0.,-2.46473488855316E-16));
#4480=DIRECTION('',(1.,0.,-2.46473488855316E-16));
#4481=DIRECTION('',(1.,0.,-2.46473488855316E-16));
#4482=DIRECTION('',(0.,1.,0.));
#4483=DIRECTION('center_axis',(-0.866025403784438,0.,0.500000000000001));
#4484=DIRECTION('ref_axis',(0.500000000000001,0.,0.866025403784438));
#4485=DIRECTION('',(0.500000000000001,0.,0.866025403784438));
#4486=DIRECTION('',(0.500000000000001,0.,0.866025403784438));
#4487=DIRECTION('',(0.500000000000001,0.,0.866025403784438));
#4488=DIRECTION('',(0.,1.,0.));
#4489=DIRECTION('center_axis',(-0.866025403784439,0.,-0.5));
#4490=DIRECTION('ref_axis',(-0.5,0.,0.866025403784439));
#4491=DIRECTION('',(-0.5,0.,0.866025403784439));
#4492=DIRECTION('',(-0.5,0.,0.866025403784439));
#4493=DIRECTION('',(-0.5,0.,0.866025403784439));
#4494=DIRECTION('',(0.,1.,0.));
#4495=DIRECTION('center_axis',(0.,0.,-1.));
#4496=DIRECTION('ref_axis',(-1.,0.,0.));
#4497=DIRECTION('',(-1.,0.,0.));
#4498=DIRECTION('',(-1.,0.,0.));
#4499=DIRECTION('',(-1.,0.,0.));
#4500=DIRECTION('',(0.,1.,0.));
#4501=DIRECTION('center_axis',(0.866025403784438,0.,-0.500000000000001));
#4502=DIRECTION('ref_axis',(-0.500000000000001,0.,-0.866025403784438));
#4503=DIRECTION('',(-0.500000000000001,0.,-0.866025403784438));
#4504=DIRECTION('',(-0.500000000000001,0.,-0.866025403784438));
#4505=DIRECTION('',(-0.500000000000001,0.,-0.866025403784438));
#4506=DIRECTION('center_axis',(0.,1.,0.));
#4507=DIRECTION('ref_axis',(0.,0.,1.));
#4508=DIRECTION('center_axis',(0.,1.,0.));
#4509=DIRECTION('ref_axis',(0.,0.,1.));
#4510=DIRECTION('center_axis',(0.,1.,0.));
#4511=DIRECTION('ref_axis',(0.,0.,1.));
#4512=DIRECTION('center_axis',(0.,1.,0.));
#4513=DIRECTION('ref_axis',(0.,0.,1.));
#4514=DIRECTION('center_axis',(0.,1.,0.));
#4515=DIRECTION('ref_axis',(0.,0.,1.));
#4516=DIRECTION('center_axis',(0.,1.,0.));
#4517=DIRECTION('ref_axis',(0.,0.,1.));
#4518=DIRECTION('center_axis',(0.,1.,0.));
#4519=DIRECTION('ref_axis',(0.,0.,1.));
#4520=DIRECTION('center_axis',(0.,0.,-1.));
#4521=DIRECTION('ref_axis',(-1.,0.,0.));
#4522=DIRECTION('center_axis',(0.,0.,-1.));
#4523=DIRECTION('ref_axis',(-1.,0.,0.));
#4524=DIRECTION('center_axis',(0.,-1.0842021724855E-16,-1.));
#4525=DIRECTION('ref_axis',(0.,-1.,1.0842021724855E-16));
#4526=DIRECTION('center_axis',(0.,0.,-1.));
#4527=DIRECTION('ref_axis',(-1.,0.,0.));
#4528=DIRECTION('center_axis',(0.,0.,1.));
#4529=DIRECTION('ref_axis',(1.,0.,0.));
#4530=DIRECTION('center_axis',(0.,3.61400724161835E-17,-1.));
#4531=DIRECTION('ref_axis',(0.,1.,3.61400724161835E-17));
#4532=DIRECTION('center_axis',(0.,-5.42101086242747E-16,-1.));
#4533=DIRECTION('ref_axis',(0.,1.,-5.42101086242747E-16));
#4534=DIRECTION('center_axis',(0.,0.,1.));
#4535=DIRECTION('ref_axis',(1.,0.,0.));
#4536=DIRECTION('center_axis',(0.,0.,1.));
#4537=DIRECTION('ref_axis',(1.,0.,0.));
#4538=DIRECTION('axis',(0.,0.,1.));
#4539=DIRECTION('refdir',(1.,0.,0.));
#4540=DIRECTION('center_axis',(0.,6.83705130257469E-33,1.));
#4541=DIRECTION('ref_axis',(1.,0.,0.));
#4542=DIRECTION('center_axis',(-1.34131666839389E-70,6.83705130257469E-33,
1.));
#4543=DIRECTION('ref_axis',(1.,0.,0.));
#4544=DIRECTION('',(0.,6.83705130257469E-33,1.));
#4545=DIRECTION('center_axis',(0.,-6.83705130257469E-33,-1.));
#4546=DIRECTION('ref_axis',(-1.,0.,0.));
#4547=DIRECTION('center_axis',(0.,6.83705130257469E-33,1.));
#4548=DIRECTION('ref_axis',(1.,0.,0.));
#4549=DIRECTION('center_axis',(0.,6.83705130257469E-33,1.));
#4550=DIRECTION('ref_axis',(1.,0.,0.));
#4551=DIRECTION('',(0.,6.83705130257469E-33,1.));
#4552=DIRECTION('center_axis',(-1.34131666839389E-70,6.83705130257469E-33,
1.));
#4553=DIRECTION('ref_axis',(1.,0.,0.));
#4554=DIRECTION('',(0.,6.83705130257469E-33,1.));
#4555=DIRECTION('center_axis',(0.,6.83705130257469E-33,1.));
#4556=DIRECTION('ref_axis',(1.,0.,0.));
#4557=DIRECTION('center_axis',(0.,6.83705130257469E-33,1.));
#4558=DIRECTION('ref_axis',(1.,0.,0.));
#4559=DIRECTION('',(0.,6.83705130257469E-33,1.));
#4560=DIRECTION('center_axis',(-1.34131666839389E-70,6.83705130257469E-33,
1.));
#4561=DIRECTION('ref_axis',(1.,0.,0.));
#4562=DIRECTION('',(0.,-6.83705130257469E-33,-1.));
#4563=DIRECTION('center_axis',(1.34131666839389E-70,-6.83705130257469E-33,
-1.));
#4564=DIRECTION('ref_axis',(-1.,-1.96183502073295E-38,0.));
#4565=DIRECTION('',(1.96183502073296E-38,1.,6.83705130257469E-33));
#4566=DIRECTION('center_axis',(0.,-6.83705130257469E-33,-1.));
#4567=DIRECTION('ref_axis',(-1.,0.,0.));
#4568=DIRECTION('',(1.96183502073296E-38,1.,6.83705130257469E-33));
#4569=DIRECTION('center_axis',(0.,-6.83705130257469E-33,-1.));
#4570=DIRECTION('ref_axis',(-1.,0.,0.));
#4571=DIRECTION('',(-1.96183502143475E-38,-1.,1.19262238973405E-16));
#4572=DIRECTION('center_axis',(0.,-6.83705130257469E-33,-1.));
#4573=DIRECTION('ref_axis',(-1.,0.,0.));
#4574=DIRECTION('center_axis',(1.34131666839389E-70,-6.83705130257469E-33,
-1.));
#4575=DIRECTION('ref_axis',(-1.,-1.96183502073295E-38,0.));
#4576=DIRECTION('center_axis',(0.,6.83705130257469E-33,1.));
#4577=DIRECTION('ref_axis',(-1.,0.,0.));
#4578=DIRECTION('',(1.96183502073296E-38,1.,6.83705130257469E-33));
#4579=DIRECTION('center_axis',(0.,6.83705130257469E-33,1.));
#4580=DIRECTION('ref_axis',(-1.,0.,0.));
#4581=DIRECTION('',(1.96183502073296E-38,1.,6.83705130257469E-33));
#4582=DIRECTION('center_axis',(0.,6.83705130257469E-33,1.));
#4583=DIRECTION('ref_axis',(-1.,1.38777878078145E-15,-9.4883147208273E-48));
#4584=DIRECTION('',(1.96183502073296E-38,1.,6.83705130257469E-33));
#4585=DIRECTION('center_axis',(-1.,-1.96183502073295E-38,1.34131666839389E-70));
#4586=DIRECTION('ref_axis',(0.,6.83705130257469E-33,1.));
#4587=DIRECTION('center_axis',(1.,1.96183502073295E-38,-1.34131666839389E-70));
#4588=DIRECTION('ref_axis',(0.,-6.83705130257469E-33,-1.));
#4589=DIRECTION('',(0.,6.83705130257469E-33,1.));
#4590=DIRECTION('',(0.,6.83705130257469E-33,1.));
#4591=DIRECTION('center_axis',(1.,1.96183502073295E-38,-1.34131666839389E-70));
#4592=DIRECTION('ref_axis',(0.,-6.83705130257469E-33,-1.));
#4593=DIRECTION('',(0.,-6.83705130257469E-33,-1.));
#4594=DIRECTION('',(0.,6.83705130257469E-33,1.));
#4595=DIRECTION('center_axis',(0.,-6.83705130257469E-33,-1.));
#4596=DIRECTION('ref_axis',(-1.,0.,0.));
#4597=DIRECTION('center_axis',(0.,6.83705130257469E-33,1.));
#4598=DIRECTION('ref_axis',(1.,0.,0.));
#4599=DIRECTION('center_axis',(0.,6.83705130257469E-33,1.));
#4600=DIRECTION('ref_axis',(1.,0.,0.));
#4601=DIRECTION('axis',(0.,0.,1.));
#4602=DIRECTION('refdir',(1.,0.,0.));
#4603=DIRECTION('center_axis',(0.,0.,1.));
#4604=DIRECTION('ref_axis',(-1.,0.,0.));
#4605=DIRECTION('center_axis',(0.,0.,1.));
#4606=DIRECTION('ref_axis',(1.,0.,0.));
#4607=DIRECTION('',(0.,0.,-1.));
#4608=DIRECTION('center_axis',(0.,0.,1.));
#4609=DIRECTION('ref_axis',(1.,0.,0.));
#4610=DIRECTION('center_axis',(0.,0.,-1.));
#4611=DIRECTION('ref_axis',(-1.,0.,0.));
#4612=DIRECTION('center_axis',(0.,0.,1.));
#4613=DIRECTION('ref_axis',(1.,0.,0.));
#4614=DIRECTION('',(0.,0.,1.));
#4615=DIRECTION('center_axis',(0.,0.,1.));
#4616=DIRECTION('ref_axis',(1.,0.,0.));
#4617=DIRECTION('center_axis',(0.,0.,-1.));
#4618=DIRECTION('ref_axis',(-1.,0.,0.));
#4619=DIRECTION('center_axis',(0.,0.,1.));
#4620=DIRECTION('ref_axis',(1.,0.,0.));
#4621=DIRECTION('',(0.,0.,1.));
#4622=DIRECTION('center_axis',(0.,0.,1.));
#4623=DIRECTION('ref_axis',(1.,0.,0.));
#4624=DIRECTION('center_axis',(0.,0.,1.));
#4625=DIRECTION('ref_axis',(1.,0.,0.));
#4626=DIRECTION('center_axis',(0.,0.,1.));
#4627=DIRECTION('ref_axis',(1.,0.,0.));
#4628=DIRECTION('center_axis',(0.,0.,-1.));
#4629=DIRECTION('ref_axis',(1.,0.,0.));
#4630=DIRECTION('center_axis',(0.,0.,-1.));
#4631=DIRECTION('ref_axis',(1.,0.,0.));
#4632=DIRECTION('',(0.,0.,1.));
#4633=DIRECTION('',(1.,0.,0.));
#4634=DIRECTION('',(-9.43319339625409E-20,-2.73835548482679E-17,-1.));
#4635=DIRECTION('',(-1.,-6.67868538251071E-17,9.43319339625427E-20));
#4636=DIRECTION('',(0.,0.,1.));
#4637=DIRECTION('',(1.,0.,0.));
#4638=DIRECTION('',(0.,0.,1.));
#4639=DIRECTION('',(1.,0.,0.));
#4640=DIRECTION('',(7.04132760396821E-22,4.33680297371949E-19,-1.));
#4641=DIRECTION('',(-1.,2.16840434497101E-18,-7.0413276039682E-22));
#4642=DIRECTION('',(0.,0.,1.));
#4643=DIRECTION('',(1.,0.,0.));
#4644=DIRECTION('',(2.07363708065791E-17,7.63375089475403E-21,-1.));
#4645=DIRECTION('',(-1.,1.58909362642649E-37,-2.07363708065791E-17));
#4646=DIRECTION('',(0.,0.,1.));
#4647=DIRECTION('',(1.,0.,0.));
#4648=DIRECTION('',(-2.77555756156289E-17,-1.92067465276309E-34,1.));
#4649=DIRECTION('',(0.98735050738457,0.158552753263488,2.7404481666842E-17));
#4650=CARTESIAN_POINT('',(0.,0.,0.));
#4651=CARTESIAN_POINT('',(0.,0.,0.));
#4652=CARTESIAN_POINT('Origin',(26.,-116.5,7.));
#4653=CARTESIAN_POINT('',(28.,-116.5,7.));
#4654=CARTESIAN_POINT('Origin',(26.,-116.5,7.));
#4655=CARTESIAN_POINT('',(28.,-116.5,2.));
#4656=CARTESIAN_POINT('',(28.,-116.5,7.));
#4657=CARTESIAN_POINT('Origin',(26.,-116.5,2.));
#4658=CARTESIAN_POINT('Origin',(26.,-116.5,7.));
#4659=CARTESIAN_POINT('',(28.,-116.5,-2.));
#4660=CARTESIAN_POINT('Origin',(26.,-116.5,-2.));
#4661=CARTESIAN_POINT('',(28.,-116.5,-7.));
#4662=CARTESIAN_POINT('',(28.,-116.5,7.));
#4663=CARTESIAN_POINT('Origin',(26.,-116.5,-7.));
#4664=CARTESIAN_POINT('Origin',(5.,-15.2931109241333,-7.));
#4665=CARTESIAN_POINT('',(3.,-15.2931109241333,-7.));
#4666=CARTESIAN_POINT('Origin',(5.,-15.2931109241333,-7.));
#4667=CARTESIAN_POINT('',(3.,-15.2931109241333,-5.));
#4668=CARTESIAN_POINT('',(3.,-15.2931109241333,-7.));
#4669=CARTESIAN_POINT('Origin',(5.,-15.2931109241333,-5.));
#4670=CARTESIAN_POINT('Origin',(5.,-15.2931109241333,-7.));
#4671=CARTESIAN_POINT('',(3.,-15.2931109241333,5.));
#4672=CARTESIAN_POINT('Origin',(5.,-15.2931109241333,5.));
#4673=CARTESIAN_POINT('',(3.,-15.2931109241333,7.));
#4674=CARTESIAN_POINT('',(3.,-15.2931109241333,-7.));
#4675=CARTESIAN_POINT('Origin',(5.,-15.2931109241333,7.));
#4676=CARTESIAN_POINT('Origin',(32.,-120.,7.));
#4677=CARTESIAN_POINT('',(23.5,-120.,-7.));
#4678=CARTESIAN_POINT('',(28.5,-120.,-7.));
#4679=CARTESIAN_POINT('',(32.,-120.,-7.));
#4680=CARTESIAN_POINT('',(28.5,-120.,-2.));
#4681=CARTESIAN_POINT('',(28.5,-120.,7.));
#4682=CARTESIAN_POINT('',(23.5,-120.,-2.));
#4683=CARTESIAN_POINT('',(32.,-120.,-2.));
#4684=CARTESIAN_POINT('',(23.5,-120.,7.));
#4685=CARTESIAN_POINT('Origin',(0.,0.,7.));
#4686=CARTESIAN_POINT('',(32.,-38.136114963014,-5.));
#4687=CARTESIAN_POINT('',(0.,0.,-5.));
#4688=CARTESIAN_POINT('',(32.,-38.136114963014,-5.));
#4689=CARTESIAN_POINT('',(32.,-38.136114963014,-7.));
#4690=CARTESIAN_POINT('',(32.,-38.136114963014,7.));
#4691=CARTESIAN_POINT('',(0.,0.,-7.));
#4692=CARTESIAN_POINT('',(0.,0.,-7.));
#4693=CARTESIAN_POINT('',(0.,0.,7.));
#4694=CARTESIAN_POINT('Origin',(0.,0.,7.));
#4695=CARTESIAN_POINT('',(23.5,-120.,7.));
#4696=CARTESIAN_POINT('',(28.5,-120.,7.));
#4697=CARTESIAN_POINT('',(32.,-120.,7.));
#4698=CARTESIAN_POINT('',(32.,-116.5,7.));
#4699=CARTESIAN_POINT('Origin',(28.5,-116.5,7.));
#4700=CARTESIAN_POINT('',(32.,-38.136114963014,7.));
#4701=CARTESIAN_POINT('',(32.,-38.136114963014,7.));
#4702=CARTESIAN_POINT('',(0.,0.,7.));
#4703=CARTESIAN_POINT('',(0.,0.,7.));
#4704=CARTESIAN_POINT('',(0.,5.,7.));
#4705=CARTESIAN_POINT('',(0.,0.,7.));
#4706=CARTESIAN_POINT('',(5.,5.,7.));
#4707=CARTESIAN_POINT('',(0.,5.,7.));
#4708=CARTESIAN_POINT('',(5.,9.,7.));
#4709=CARTESIAN_POINT('',(5.,40.,7.));
#4710=CARTESIAN_POINT('',(5.,11.,7.));
#4711=CARTESIAN_POINT('Origin',(5.00000000000001,10.,7.));
#4712=CARTESIAN_POINT('',(5.,12.5,7.));
#4713=CARTESIAN_POINT('',(5.,40.,7.));
#4714=CARTESIAN_POINT('',(5.,14.5,7.));
#4715=CARTESIAN_POINT('Origin',(5.00000000000001,13.5,7.));
#4716=CARTESIAN_POINT('',(5.,16.,7.));
#4717=CARTESIAN_POINT('',(5.,40.,7.));
#4718=CARTESIAN_POINT('',(5.,18.,7.));
#4719=CARTESIAN_POINT('Origin',(5.00000000000001,17.,7.));
#4720=CARTESIAN_POINT('',(5.,19.5,7.));
#4721=CARTESIAN_POINT('',(5.,40.,7.));
#4722=CARTESIAN_POINT('',(5.,21.5,7.));
#4723=CARTESIAN_POINT('Origin',(5.00000000000001,20.5,7.));
#4724=CARTESIAN_POINT('',(5.,23.,7.));
#4725=CARTESIAN_POINT('',(5.,40.,7.));
#4726=CARTESIAN_POINT('',(5.,25.,7.));
#4727=CARTESIAN_POINT('Origin',(5.00000000000001,24.,7.));
#4728=CARTESIAN_POINT('',(5.,26.5,7.));
#4729=CARTESIAN_POINT('',(5.,40.,7.));
#4730=CARTESIAN_POINT('',(5.,28.5,7.));
#4731=CARTESIAN_POINT('Origin',(5.00000000000001,27.5,7.));
#4732=CARTESIAN_POINT('',(5.,30.,7.));
#4733=CARTESIAN_POINT('',(5.,40.,7.));
#4734=CARTESIAN_POINT('',(5.,32.,7.));
#4735=CARTESIAN_POINT('Origin',(5.00000000000001,31.,7.));
#4736=CARTESIAN_POINT('',(5.,33.5,7.));
#4737=CARTESIAN_POINT('',(5.,40.,7.));
#4738=CARTESIAN_POINT('',(5.,35.5,7.));
#4739=CARTESIAN_POINT('Origin',(5.00000000000001,34.5,7.));
#4740=CARTESIAN_POINT('',(5.,37.,7.));
#4741=CARTESIAN_POINT('',(5.,40.,7.));
#4742=CARTESIAN_POINT('',(5.,39.,7.));
#4743=CARTESIAN_POINT('Origin',(5.,38.,7.));
#4744=CARTESIAN_POINT('',(5.,40.,7.));
#4745=CARTESIAN_POINT('',(5.,40.,7.));
#4746=CARTESIAN_POINT('',(-5.,40.,7.));
#4747=CARTESIAN_POINT('',(0.,40.,7.));
#4748=CARTESIAN_POINT('',(-15.705120202908,0.0479475016143677,7.));
#4749=CARTESIAN_POINT('',(-5.,40.,7.));
#4750=CARTESIAN_POINT('',(20.,-42.5037577742085,7.));
#4751=CARTESIAN_POINT('',(-15.705120202908,0.0479475016143677,7.));
#4752=CARTESIAN_POINT('',(20.,-116.5,7.));
#4753=CARTESIAN_POINT('',(20.,-42.5037577742085,7.));
#4754=CARTESIAN_POINT('Origin',(23.5,-116.5,7.));
#4755=CARTESIAN_POINT('Origin',(0.,0.,-7.));
#4756=CARTESIAN_POINT('',(32.,-116.5,-7.));
#4757=CARTESIAN_POINT('',(32.,-38.136114963014,-7.));
#4758=CARTESIAN_POINT('Origin',(28.5,-116.5,-7.));
#4759=CARTESIAN_POINT('',(20.,-116.5,-7.));
#4760=CARTESIAN_POINT('Origin',(23.5,-116.5,-7.));
#4761=CARTESIAN_POINT('',(20.,-42.5037577742085,-7.));
#4762=CARTESIAN_POINT('',(20.,-42.5037577742085,-7.));
#4763=CARTESIAN_POINT('',(-15.705120202908,0.0479475016143677,-7.));
#4764=CARTESIAN_POINT('',(-15.705120202908,0.0479475016143677,-7.));
#4765=CARTESIAN_POINT('',(-5.,40.,-7.));
#4766=CARTESIAN_POINT('',(-5.,40.,-7.));
#4767=CARTESIAN_POINT('',(5.,40.,-7.));
#4768=CARTESIAN_POINT('',(0.,40.,-7.));
#4769=CARTESIAN_POINT('',(5.,39.,-7.));
#4770=CARTESIAN_POINT('',(5.,40.,-7.));
#4771=CARTESIAN_POINT('',(5.,37.,-7.));
#4772=CARTESIAN_POINT('Origin',(5.,38.,-7.));
#4773=CARTESIAN_POINT('',(5.,35.5,-7.));
#4774=CARTESIAN_POINT('',(5.,40.,-7.));
#4775=CARTESIAN_POINT('',(5.,33.5,-7.));
#4776=CARTESIAN_POINT('Origin',(5.00000000000001,34.5,-7.));
#4777=CARTESIAN_POINT('',(5.,32.,-7.));
#4778=CARTESIAN_POINT('',(5.,40.,-7.));
#4779=CARTESIAN_POINT('',(5.,30.,-7.));
#4780=CARTESIAN_POINT('Origin',(5.00000000000001,31.,-7.));
#4781=CARTESIAN_POINT('',(5.,28.5,-7.));
#4782=CARTESIAN_POINT('',(5.,40.,-7.));
#4783=CARTESIAN_POINT('',(5.,26.5,-7.));
#4784=CARTESIAN_POINT('Origin',(5.00000000000001,27.5,-7.));
#4785=CARTESIAN_POINT('',(5.,25.,-7.));
#4786=CARTESIAN_POINT('',(5.,40.,-7.));
#4787=CARTESIAN_POINT('',(5.,23.,-7.));
#4788=CARTESIAN_POINT('Origin',(5.00000000000001,24.,-7.));
#4789=CARTESIAN_POINT('',(5.,21.5,-7.));
#4790=CARTESIAN_POINT('',(5.,40.,-7.));
#4791=CARTESIAN_POINT('',(5.,19.5,-7.));
#4792=CARTESIAN_POINT('Origin',(5.00000000000001,20.5,-7.));
#4793=CARTESIAN_POINT('',(5.,18.,-7.));
#4794=CARTESIAN_POINT('',(5.,40.,-7.));
#4795=CARTESIAN_POINT('',(5.,16.,-7.));
#4796=CARTESIAN_POINT('Origin',(5.00000000000001,17.,-7.));
#4797=CARTESIAN_POINT('',(5.,14.5,-7.));
#4798=CARTESIAN_POINT('',(5.,40.,-7.));
#4799=CARTESIAN_POINT('',(5.,12.5,-7.));
#4800=CARTESIAN_POINT('Origin',(5.00000000000001,13.5,-7.));
#4801=CARTESIAN_POINT('',(5.,11.,-7.));
#4802=CARTESIAN_POINT('',(5.,40.,-7.));
#4803=CARTESIAN_POINT('',(5.,9.,-7.));
#4804=CARTESIAN_POINT('Origin',(5.00000000000001,10.,-7.));
#4805=CARTESIAN_POINT('',(5.,5.,-7.));
#4806=CARTESIAN_POINT('',(5.,40.,-7.));
#4807=CARTESIAN_POINT('',(0.,5.,-7.));
#4808=CARTESIAN_POINT('',(0.,5.,-7.));
#4809=CARTESIAN_POINT('',(0.,0.,-7.));
#4810=CARTESIAN_POINT('Origin',(5.,40.,7.));
#4811=CARTESIAN_POINT('',(5.,33.5,-7.));
#4812=CARTESIAN_POINT('',(5.,32.,-7.));
#4813=CARTESIAN_POINT('Origin',(5.,40.,7.));
#4814=CARTESIAN_POINT('',(5.,30.,-7.));
#4815=CARTESIAN_POINT('',(5.,28.5,-7.));
#4816=CARTESIAN_POINT('Origin',(5.,40.,7.));
#4817=CARTESIAN_POINT('',(5.,26.5,-7.));
#4818=CARTESIAN_POINT('',(5.,25.,-7.));
#4819=CARTESIAN_POINT('Origin',(5.,40.,7.));
#4820=CARTESIAN_POINT('',(5.,23.,-7.));
#4821=CARTESIAN_POINT('',(5.,21.5,-7.));
#4822=CARTESIAN_POINT('Origin',(5.,40.,7.));
#4823=CARTESIAN_POINT('',(5.,19.5,-7.));
#4824=CARTESIAN_POINT('',(5.,18.,-7.));
#4825=CARTESIAN_POINT('Origin',(5.,40.,7.));
#4826=CARTESIAN_POINT('',(5.,16.,-7.));
#4827=CARTESIAN_POINT('',(5.,14.5,-7.));
#4828=CARTESIAN_POINT('Origin',(5.,40.,7.));
#4829=CARTESIAN_POINT('',(5.,12.5,-7.));
#4830=CARTESIAN_POINT('',(5.,11.,-7.));
#4831=CARTESIAN_POINT('Origin',(5.,40.,7.));
#4832=CARTESIAN_POINT('',(5.,9.,-7.));
#4833=CARTESIAN_POINT('',(5.,5.,7.));
#4834=CARTESIAN_POINT('Origin',(5.,40.,7.));
#4835=CARTESIAN_POINT('',(5.,35.5,-7.));
#4836=CARTESIAN_POINT('',(5.,37.,-7.));
#4837=CARTESIAN_POINT('Origin',(0.,0.,7.));
#4838=CARTESIAN_POINT('',(0.,5.,7.));
#4839=CARTESIAN_POINT('',(0.,0.,5.));
#4840=CARTESIAN_POINT('',(0.,0.,7.));
#4841=CARTESIAN_POINT('',(0.,0.,-5.));
#4842=CARTESIAN_POINT('Origin',(0.,0.,7.));
#4843=CARTESIAN_POINT('',(32.,-38.136114963014,5.));
#4844=CARTESIAN_POINT('',(32.,-38.136114963014,7.));
#4845=CARTESIAN_POINT('',(32.,-38.136114963014,5.));
#4846=CARTESIAN_POINT('Origin',(0.,40.,7.));
#4847=CARTESIAN_POINT('',(-5.,40.,7.));
#4848=CARTESIAN_POINT('',(5.,40.,7.));
#4849=CARTESIAN_POINT('Origin',(-5.,40.,7.));
#4850=CARTESIAN_POINT('',(-15.705120202908,0.0479475016143677,7.));
#4851=CARTESIAN_POINT('Origin',(-15.705120202908,0.0479475016143677,7.));
#4852=CARTESIAN_POINT('',(-9.19253331742767,-7.71345131623856,-5.));
#4853=CARTESIAN_POINT('',(-9.19253331742767,-7.71345131623856,5.));
#4854=CARTESIAN_POINT('',(-9.19253331742767,-7.71345131623856,-5.));
#4855=CARTESIAN_POINT('',(20.,-42.5037577742085,5.));
#4856=CARTESIAN_POINT('',(-9.19253331742767,-7.71345131623856,5.));
#4857=CARTESIAN_POINT('',(20.,-42.5037577742085,7.));
#4858=CARTESIAN_POINT('',(20.,-42.5037577742085,-5.));
#4859=CARTESIAN_POINT('',(20.,-42.5037577742085,7.));
#4860=CARTESIAN_POINT('',(-9.19253331742767,-7.71345131623856,-5.));
#4861=CARTESIAN_POINT('Origin',(20.,-42.5037577742085,7.));
#4862=CARTESIAN_POINT('',(20.,-50.,2.));
#4863=CARTESIAN_POINT('',(20.,-116.5,2.));
#4864=CARTESIAN_POINT('',(20.,-42.5037577742085,2.));
#4865=CARTESIAN_POINT('',(20.,-116.5,7.));
#4866=CARTESIAN_POINT('',(20.,-42.5037577742085,-5.));
#4867=CARTESIAN_POINT('',(20.,-116.5,-2.));
#4868=CARTESIAN_POINT('',(20.,-116.5,7.));
#4869=CARTESIAN_POINT('',(20.,-50.,-2.));
#4870=CARTESIAN_POINT('',(20.,-42.5037577742085,-2.));
#4871=CARTESIAN_POINT('',(20.,-50.,7.));
#4872=CARTESIAN_POINT('Origin',(32.,-120.,7.));
#4873=CARTESIAN_POINT('',(28.5,-120.,2.));
#4874=CARTESIAN_POINT('',(23.5,-120.,2.));
#4875=CARTESIAN_POINT('',(32.,-120.,2.));
#4876=CARTESIAN_POINT('',(28.5,-120.,7.));
#4877=CARTESIAN_POINT('',(23.5,-120.,7.));
#4878=CARTESIAN_POINT('Origin',(32.,-38.136114963014,7.));
#4879=CARTESIAN_POINT('',(32.,-116.5,2.));
#4880=CARTESIAN_POINT('',(32.,-116.5,7.));
#4881=CARTESIAN_POINT('',(32.,-50.,2.));
#4882=CARTESIAN_POINT('',(32.,-120.,2.));
#4883=CARTESIAN_POINT('',(32.,-50.,-2.));
#4884=CARTESIAN_POINT('',(32.,-50.,-2.));
#4885=CARTESIAN_POINT('',(32.,-116.5,-2.));
#4886=CARTESIAN_POINT('',(32.,-120.,-2.));
#4887=CARTESIAN_POINT('',(32.,-116.5,7.));
#4888=CARTESIAN_POINT('',(32.,-38.136114963014,-5.));
#4889=CARTESIAN_POINT('Origin',(0.,5.,7.));
#4890=CARTESIAN_POINT('Origin',(5.,40.,7.));
#4891=CARTESIAN_POINT('',(5.,39.,-7.));
#4892=CARTESIAN_POINT('Origin',(5.,38.,-7.));
#4893=CARTESIAN_POINT('Origin',(5.00000000000001,10.,-7.));
#4894=CARTESIAN_POINT('Origin',(5.00000000000001,13.5,-7.));
#4895=CARTESIAN_POINT('Origin',(5.00000000000001,17.,-7.));
#4896=CARTESIAN_POINT('Origin',(5.00000000000001,20.5,-7.));
#4897=CARTESIAN_POINT('Origin',(5.00000000000001,24.,-7.));
#4898=CARTESIAN_POINT('Origin',(5.00000000000001,27.5,-7.));
#4899=CARTESIAN_POINT('Origin',(5.00000000000001,31.,-7.));
#4900=CARTESIAN_POINT('Origin',(5.00000000000001,34.5,-7.));
#4901=CARTESIAN_POINT('Origin',(20.,-42.5037577742085,-5.));
#4902=CARTESIAN_POINT('',(20.,-42.5037577742085,5.));
#4903=CARTESIAN_POINT('',(20.,-42.5037577742085,-5.));
#4904=CARTESIAN_POINT('Origin',(0.,0.,-5.));
#4905=CARTESIAN_POINT('',(0.,0.,5.));
#4906=CARTESIAN_POINT('',(0.,0.,-5.));
#4907=CARTESIAN_POINT('Origin',(0.,0.,-5.));
#4908=CARTESIAN_POINT('Origin',(0.,0.,5.));
#4909=CARTESIAN_POINT('Origin',(32.,-120.,2.));
#4910=CARTESIAN_POINT('Origin',(28.5,-116.5,2.));
#4911=CARTESIAN_POINT('Origin',(23.5,-116.5,2.));
#4912=CARTESIAN_POINT('',(32.,-50.,2.));
#4913=CARTESIAN_POINT('Origin',(32.,-120.,-2.));
#4914=CARTESIAN_POINT('Origin',(28.5,-116.5,-2.));
#4915=CARTESIAN_POINT('',(32.,-50.,-2.));
#4916=CARTESIAN_POINT('Origin',(23.5,-116.5,-2.));
#4917=CARTESIAN_POINT('Origin',(32.,-50.,-2.));
#4918=CARTESIAN_POINT('Origin',(28.5,-116.5,7.));
#4919=CARTESIAN_POINT('Origin',(28.5,-116.5,7.));
#4920=CARTESIAN_POINT('Origin',(23.5,-116.5,7.));
#4921=CARTESIAN_POINT('Origin',(23.5,-116.5,7.));
#4922=CARTESIAN_POINT('',(0.,0.,0.));
#4923=CARTESIAN_POINT('Origin',(26.,-116.5,-7.));
#4924=CARTESIAN_POINT('',(24.,-116.5,-7.));
#4925=CARTESIAN_POINT('Origin',(26.,-116.5,-7.));
#4926=CARTESIAN_POINT('',(24.,-116.5,-2.));
#4927=CARTESIAN_POINT('',(24.,-116.5,-7.));
#4928=CARTESIAN_POINT('Origin',(26.,-116.5,-2.));
#4929=CARTESIAN_POINT('Origin',(26.,-116.5,-7.));
#4930=CARTESIAN_POINT('',(24.,-116.5,2.));
#4931=CARTESIAN_POINT('Origin',(26.,-116.5,2.));
#4932=CARTESIAN_POINT('',(24.,-116.5,7.));
#4933=CARTESIAN_POINT('',(24.,-116.5,-7.));
#4934=CARTESIAN_POINT('Origin',(26.,-116.5,7.));
#4935=CARTESIAN_POINT('Origin',(5.,-15.2931109241333,7.));
#4936=CARTESIAN_POINT('',(7.,-15.2931109241333,5.));
#4937=CARTESIAN_POINT('Origin',(5.,-15.2931109241333,5.));
#4938=CARTESIAN_POINT('',(7.,-15.2931109241333,-5.));
#4939=CARTESIAN_POINT('',(7.,-15.2931109241333,7.));
#4940=CARTESIAN_POINT('Origin',(5.,-15.2931109241333,-5.));
#4941=CARTESIAN_POINT('Origin',(0.,0.,7.));
#4942=CARTESIAN_POINT('',(20.,-42.5037577742085,7.));
#4943=CARTESIAN_POINT('',(20.,-116.5,7.));
#4944=CARTESIAN_POINT('',(20.,-42.5037577742085,7.));
#4945=CARTESIAN_POINT('',(23.5,-120.,7.));
#4946=CARTESIAN_POINT('Origin',(23.5,-116.5,7.));
#4947=CARTESIAN_POINT('',(28.5,-120.,7.));
#4948=CARTESIAN_POINT('',(32.,-120.,7.));
#4949=CARTESIAN_POINT('',(32.,-116.5,7.));
#4950=CARTESIAN_POINT('Origin',(28.5,-116.5,7.));
#4951=CARTESIAN_POINT('',(32.,-38.136114963014,7.));
#4952=CARTESIAN_POINT('',(32.,-38.136114963014,7.));
#4953=CARTESIAN_POINT('',(20.,-42.5037577742085,7.));
#4954=CARTESIAN_POINT('Origin',(32.,-120.,7.));
#4955=CARTESIAN_POINT('',(23.5,-120.,2.));
#4956=CARTESIAN_POINT('',(23.5,-120.,7.));
#4957=CARTESIAN_POINT('',(28.5,-120.,2.));
#4958=CARTESIAN_POINT('',(-15.705120202908,-120.,2.));
#4959=CARTESIAN_POINT('',(28.5,-120.,7.));
#4960=CARTESIAN_POINT('Origin',(-15.705120202908,0.0479475016143815,7.));
#4961=CARTESIAN_POINT('',(-9.19253331742767,-7.71345131623855,7.));
#4962=CARTESIAN_POINT('',(-9.19253331742767,-7.71345131623855,5.));
#4963=CARTESIAN_POINT('',(-9.19253331742767,-7.71345131623855,7.000012));
#4964=CARTESIAN_POINT('',(-15.705120202908,0.0479475016143815,7.));
#4965=CARTESIAN_POINT('',(-15.705120202908,0.0479475016143815,7.));
#4966=CARTESIAN_POINT('',(-15.705120202908,0.0479475016143843,-7.));
#4967=CARTESIAN_POINT('',(-15.705120202908,0.0479475016143815,7.));
#4968=CARTESIAN_POINT('',(-9.19253331742767,-7.71345131623855,-7.));
#4969=CARTESIAN_POINT('',(-15.705120202908,0.0479475016143815,-7.));
#4970=CARTESIAN_POINT('',(-9.19253331742767,-7.71345131623855,-5.));
#4971=CARTESIAN_POINT('',(-9.19253331742767,-7.71345131623855,-7.000012));
#4972=CARTESIAN_POINT('',(20.,-42.5037577742085,-5.));
#4973=CARTESIAN_POINT('',(-9.19253331742767,-7.71345131623855,-5.));
#4974=CARTESIAN_POINT('',(20.,-42.5037577742085,5.));
#4975=CARTESIAN_POINT('',(20.,-42.5037577742085,7.));
#4976=CARTESIAN_POINT('',(-9.19253331742767,-7.71345131623855,5.));
#4977=CARTESIAN_POINT('Origin',(0.,0.,7.));
#4978=CARTESIAN_POINT('',(0.,0.,7.));
#4979=CARTESIAN_POINT('',(0.,0.,7.));
#4980=CARTESIAN_POINT('',(0.,5.,7.));
#4981=CARTESIAN_POINT('',(0.,0.,7.));
#4982=CARTESIAN_POINT('',(5.,5.,7.));
#4983=CARTESIAN_POINT('',(0.,5.,7.));
#4984=CARTESIAN_POINT('',(5.,9.,7.));
#4985=CARTESIAN_POINT('',(5.,40.,7.));
#4986=CARTESIAN_POINT('',(5.,11.,7.));
#4987=CARTESIAN_POINT('Origin',(5.00000000000001,10.,7.));
#4988=CARTESIAN_POINT('',(5.,12.5,7.));
#4989=CARTESIAN_POINT('',(5.,40.,7.));
#4990=CARTESIAN_POINT('',(5.,14.5,7.));
#4991=CARTESIAN_POINT('Origin',(5.00000000000001,13.5,7.));
#4992=CARTESIAN_POINT('',(5.,16.,7.));
#4993=CARTESIAN_POINT('',(5.,40.,7.));
#4994=CARTESIAN_POINT('',(5.,18.,7.));
#4995=CARTESIAN_POINT('Origin',(5.00000000000001,17.,7.));
#4996=CARTESIAN_POINT('',(5.,19.5,7.));
#4997=CARTESIAN_POINT('',(5.,40.,7.));
#4998=CARTESIAN_POINT('',(5.,21.5,7.));
#4999=CARTESIAN_POINT('Origin',(5.00000000000001,20.5,7.));
#5000=CARTESIAN_POINT('',(5.,23.,7.));
#5001=CARTESIAN_POINT('',(5.,40.,7.));
#5002=CARTESIAN_POINT('',(5.,25.,7.));
#5003=CARTESIAN_POINT('Origin',(5.00000000000001,24.,7.));
#5004=CARTESIAN_POINT('',(5.,26.5,7.));
#5005=CARTESIAN_POINT('',(5.,40.,7.));
#5006=CARTESIAN_POINT('',(5.,28.5,7.));
#5007=CARTESIAN_POINT('Origin',(5.00000000000001,27.5,7.));
#5008=CARTESIAN_POINT('',(5.,30.,7.));
#5009=CARTESIAN_POINT('',(5.,40.,7.));
#5010=CARTESIAN_POINT('',(5.,32.,7.));
#5011=CARTESIAN_POINT('Origin',(5.00000000000001,31.,7.));
#5012=CARTESIAN_POINT('',(5.,33.5,7.));
#5013=CARTESIAN_POINT('',(5.,40.,7.));
#5014=CARTESIAN_POINT('',(5.,35.5,7.));
#5015=CARTESIAN_POINT('Origin',(5.00000000000001,34.5,7.));
#5016=CARTESIAN_POINT('',(5.,37.,7.));
#5017=CARTESIAN_POINT('',(5.,40.,7.));
#5018=CARTESIAN_POINT('',(5.,39.,7.));
#5019=CARTESIAN_POINT('Origin',(5.,38.,7.));
#5020=CARTESIAN_POINT('',(5.,40.,7.));
#5021=CARTESIAN_POINT('',(5.,40.,7.));
#5022=CARTESIAN_POINT('',(-5.,40.,7.));
#5023=CARTESIAN_POINT('',(0.,40.,7.));
#5024=CARTESIAN_POINT('',(-5.,40.,7.));
#5025=CARTESIAN_POINT('Origin',(0.,0.,-7.));
#5026=CARTESIAN_POINT('',(23.5,-120.,-7.));
#5027=CARTESIAN_POINT('',(28.5,-120.,-7.));
#5028=CARTESIAN_POINT('',(32.,-120.,-7.));
#5029=CARTESIAN_POINT('',(20.,-116.5,-7.));
#5030=CARTESIAN_POINT('Origin',(23.5,-116.5,-7.));
#5031=CARTESIAN_POINT('',(20.,-42.5037577742085,-7.));
#5032=CARTESIAN_POINT('',(20.,-42.5037577742085,-7.));
#5033=CARTESIAN_POINT('',(32.,-38.136114963014,-7.));
#5034=CARTESIAN_POINT('',(20.,-42.5037577742085,-7.));
#5035=CARTESIAN_POINT('',(32.,-116.5,-7.));
#5036=CARTESIAN_POINT('',(32.,-38.136114963014,-7.));
#5037=CARTESIAN_POINT('Origin',(28.5,-116.5,-7.));
#5038=CARTESIAN_POINT('Origin',(0.,0.,7.));
#5039=CARTESIAN_POINT('',(0.,0.,5.));
#5040=CARTESIAN_POINT('',(0.,0.,-5.));
#5041=CARTESIAN_POINT('',(0.,0.,7.));
#5042=CARTESIAN_POINT('',(32.,-38.136114963014,5.));
#5043=CARTESIAN_POINT('',(32.,-38.136114963014,5.));
#5044=CARTESIAN_POINT('',(32.,-38.136114963014,-5.));
#5045=CARTESIAN_POINT('',(32.,-38.136114963014,7.));
#5046=CARTESIAN_POINT('',(32.,-38.136114963014,-5.));
#5047=CARTESIAN_POINT('Origin',(0.,0.,-7.));
#5048=CARTESIAN_POINT('',(0.,0.,-7.));
#5049=CARTESIAN_POINT('',(0.,0.,-7.));
#5050=CARTESIAN_POINT('',(-5.,40.,-7.));
#5051=CARTESIAN_POINT('',(-5.,40.,-7.));
#5052=CARTESIAN_POINT('',(5.,40.,-7.));
#5053=CARTESIAN_POINT('',(0.,40.,-7.));
#5054=CARTESIAN_POINT('',(5.,39.,-7.));
#5055=CARTESIAN_POINT('',(5.,40.,-7.));
#5056=CARTESIAN_POINT('',(5.,37.,-7.));
#5057=CARTESIAN_POINT('Origin',(5.,38.,-7.));
#5058=CARTESIAN_POINT('',(5.,35.5,-7.));
#5059=CARTESIAN_POINT('',(5.,40.,-7.));
#5060=CARTESIAN_POINT('',(5.,33.5,-7.));
#5061=CARTESIAN_POINT('Origin',(5.00000000000001,34.5,-7.));
#5062=CARTESIAN_POINT('',(5.,32.,-7.));
#5063=CARTESIAN_POINT('',(5.,40.,-7.));
#5064=CARTESIAN_POINT('',(5.,30.,-7.));
#5065=CARTESIAN_POINT('Origin',(5.00000000000001,31.,-7.));
#5066=CARTESIAN_POINT('',(5.,28.5,-7.));
#5067=CARTESIAN_POINT('',(5.,40.,-7.));
#5068=CARTESIAN_POINT('',(5.,26.5,-7.));
#5069=CARTESIAN_POINT('Origin',(5.00000000000001,27.5,-7.));
#5070=CARTESIAN_POINT('',(5.,25.,-7.));
#5071=CARTESIAN_POINT('',(5.,40.,-7.));
#5072=CARTESIAN_POINT('',(5.,23.,-7.));
#5073=CARTESIAN_POINT('Origin',(5.00000000000001,24.,-7.));
#5074=CARTESIAN_POINT('',(5.,21.5,-7.));
#5075=CARTESIAN_POINT('',(5.,40.,-7.));
#5076=CARTESIAN_POINT('',(5.,19.5,-7.));
#5077=CARTESIAN_POINT('Origin',(5.00000000000001,20.5,-7.));
#5078=CARTESIAN_POINT('',(5.,18.,-7.));
#5079=CARTESIAN_POINT('',(5.,40.,-7.));
#5080=CARTESIAN_POINT('',(5.,16.,-7.));
#5081=CARTESIAN_POINT('Origin',(5.00000000000001,17.,-7.));
#5082=CARTESIAN_POINT('',(5.,14.5,-7.));
#5083=CARTESIAN_POINT('',(5.,40.,-7.));
#5084=CARTESIAN_POINT('',(5.,12.5,-7.));
#5085=CARTESIAN_POINT('Origin',(5.00000000000001,13.5,-7.));
#5086=CARTESIAN_POINT('',(5.,11.,-7.));
#5087=CARTESIAN_POINT('',(5.,40.,-7.));
#5088=CARTESIAN_POINT('',(5.,9.,-7.));
#5089=CARTESIAN_POINT('Origin',(5.00000000000001,10.,-7.));
#5090=CARTESIAN_POINT('',(5.,5.,-7.));
#5091=CARTESIAN_POINT('',(5.,40.,-7.));
#5092=CARTESIAN_POINT('',(0.,5.,-7.));
#5093=CARTESIAN_POINT('',(0.,5.,-7.));
#5094=CARTESIAN_POINT('',(0.,0.,-7.));
#5095=CARTESIAN_POINT('Origin',(5.,40.,7.));
#5096=CARTESIAN_POINT('',(5.,33.5,-7.));
#5097=CARTESIAN_POINT('',(5.,32.,-7.));
#5098=CARTESIAN_POINT('Origin',(5.,40.,7.));
#5099=CARTESIAN_POINT('',(5.,30.,-7.));
#5100=CARTESIAN_POINT('',(5.,28.5,-7.));
#5101=CARTESIAN_POINT('Origin',(5.,40.,7.));
#5102=CARTESIAN_POINT('',(5.,26.5,-7.));
#5103=CARTESIAN_POINT('',(5.,25.,-7.));
#5104=CARTESIAN_POINT('Origin',(5.,40.,7.));
#5105=CARTESIAN_POINT('',(5.,23.,-7.));
#5106=CARTESIAN_POINT('',(5.,21.5,-7.));
#5107=CARTESIAN_POINT('Origin',(5.,40.,7.));
#5108=CARTESIAN_POINT('',(5.,19.5,-7.));
#5109=CARTESIAN_POINT('',(5.,18.,-7.));
#5110=CARTESIAN_POINT('Origin',(5.,40.,7.));
#5111=CARTESIAN_POINT('',(5.,16.,-7.));
#5112=CARTESIAN_POINT('',(5.,14.5,-7.));
#5113=CARTESIAN_POINT('Origin',(5.,40.,7.));
#5114=CARTESIAN_POINT('',(5.,12.5,-7.));
#5115=CARTESIAN_POINT('',(5.,11.,-7.));
#5116=CARTESIAN_POINT('Origin',(5.,40.,7.));
#5117=CARTESIAN_POINT('',(5.,9.,-7.));
#5118=CARTESIAN_POINT('',(5.,5.,7.));
#5119=CARTESIAN_POINT('Origin',(5.,40.,7.));
#5120=CARTESIAN_POINT('',(5.,35.5,-7.));
#5121=CARTESIAN_POINT('',(5.,37.,-7.));
#5122=CARTESIAN_POINT('Origin',(0.,0.,7.));
#5123=CARTESIAN_POINT('',(0.,5.,7.));
#5124=CARTESIAN_POINT('',(0.,0.,7.));
#5125=CARTESIAN_POINT('',(0.,0.,-7.000012));
#5126=CARTESIAN_POINT('Origin',(0.,40.,7.));
#5127=CARTESIAN_POINT('',(-5.,40.,7.));
#5128=CARTESIAN_POINT('',(5.,40.,7.));
#5129=CARTESIAN_POINT('Origin',(-5.,40.,7.));
#5130=CARTESIAN_POINT('Origin',(20.,-42.5037577742085,7.));
#5131=CARTESIAN_POINT('',(20.,-116.5,-2.));
#5132=CARTESIAN_POINT('',(20.,-116.5,7.));
#5133=CARTESIAN_POINT('',(20.,-50.,-2.));
#5134=CARTESIAN_POINT('',(20.,-42.5037577742085,-2.));
#5135=CARTESIAN_POINT('',(20.,-50.,2.));
#5136=CARTESIAN_POINT('',(20.,-50.,7.));
#5137=CARTESIAN_POINT('',(20.,-116.5,2.));
#5138=CARTESIAN_POINT('',(20.,-42.5037577742085,2.));
#5139=CARTESIAN_POINT('',(20.,-116.5,7.));
#5140=CARTESIAN_POINT('',(20.,-42.5037577742085,7.));
#5141=CARTESIAN_POINT('',(20.,-42.5037577742085,-7.000012));
#5142=CARTESIAN_POINT('Origin',(32.,-120.,7.));
#5143=CARTESIAN_POINT('',(23.5,-120.,-2.));
#5144=CARTESIAN_POINT('',(28.5,-120.,-2.));
#5145=CARTESIAN_POINT('',(-15.705120202908,-120.,-2.));
#5146=CARTESIAN_POINT('',(23.5,-120.,7.));
#5147=CARTESIAN_POINT('',(28.5,-120.,7.));
#5148=CARTESIAN_POINT('Origin',(32.,-38.136114963014,7.));
#5149=CARTESIAN_POINT('',(32.,-116.5,2.));
#5150=CARTESIAN_POINT('',(32.,-116.5,7.));
#5151=CARTESIAN_POINT('',(32.,-50.,2.));
#5152=CARTESIAN_POINT('',(32.,-120.,2.));
#5153=CARTESIAN_POINT('',(32.,-50.,-2.));
#5154=CARTESIAN_POINT('',(32.,-50.,2.));
#5155=CARTESIAN_POINT('',(32.,-116.5,-2.));
#5156=CARTESIAN_POINT('',(32.,-120.,-2.));
#5157=CARTESIAN_POINT('',(32.,-116.5,7.));
#5158=CARTESIAN_POINT('',(32.,-38.136114963014,-7.000012));
#5159=CARTESIAN_POINT('',(32.,-38.136114963014,7.));
#5160=CARTESIAN_POINT('Origin',(0.,5.,7.));
#5161=CARTESIAN_POINT('Origin',(5.,40.,7.));
#5162=CARTESIAN_POINT('',(5.,39.,-7.));
#5163=CARTESIAN_POINT('Origin',(5.,38.,-7.));
#5164=CARTESIAN_POINT('Origin',(5.00000000000001,10.,-7.));
#5165=CARTESIAN_POINT('Origin',(5.00000000000001,13.5,-7.));
#5166=CARTESIAN_POINT('Origin',(5.00000000000001,17.,-7.));
#5167=CARTESIAN_POINT('Origin',(5.00000000000001,20.5,-7.));
#5168=CARTESIAN_POINT('Origin',(5.00000000000001,24.,-7.));
#5169=CARTESIAN_POINT('Origin',(5.00000000000001,27.5,-7.));
#5170=CARTESIAN_POINT('Origin',(5.00000000000001,31.,-7.));
#5171=CARTESIAN_POINT('Origin',(5.00000000000001,34.5,-7.));
#5172=CARTESIAN_POINT('Origin',(20.,-42.5037577742085,-7.000012));
#5173=CARTESIAN_POINT('',(20.,-42.5037577742085,-5.));
#5174=CARTESIAN_POINT('Origin',(0.,0.,-7.000012));
#5175=CARTESIAN_POINT('',(0.,0.,-5.));
#5176=CARTESIAN_POINT('Origin',(0.,0.,-5.));
#5177=CARTESIAN_POINT('Origin',(20.,-42.5037577742085,7.000012));
#5178=CARTESIAN_POINT('',(20.,-42.5037577742085,5.));
#5179=CARTESIAN_POINT('Origin',(0.,0.,7.000012));
#5180=CARTESIAN_POINT('',(0.,0.,5.));
#5181=CARTESIAN_POINT('Origin',(0.,0.,5.));
#5182=CARTESIAN_POINT('Origin',(-15.705120202908,-120.,-2.));
#5183=CARTESIAN_POINT('Origin',(23.5,-116.5,-2.));
#5184=CARTESIAN_POINT('Origin',(28.5,-116.5,-2.));
#5185=CARTESIAN_POINT('',(-15.705120202908,-50.,-2.));
#5186=CARTESIAN_POINT('Origin',(-15.705120202908,-120.,2.));
#5187=CARTESIAN_POINT('Origin',(23.5,-116.5,2.));
#5188=CARTESIAN_POINT('',(-15.705120202908,-50.,2.));
#5189=CARTESIAN_POINT('Origin',(28.5,-116.5,2.));
#5190=CARTESIAN_POINT('Origin',(-15.705120202908,-50.,2.));
#5191=CARTESIAN_POINT('Origin',(23.5,-116.5,7.));
#5192=CARTESIAN_POINT('Origin',(23.5,-116.5,7.));
#5193=CARTESIAN_POINT('Origin',(28.5,-116.5,7.));
#5194=CARTESIAN_POINT('Origin',(28.5,-116.5,7.));
#5195=CARTESIAN_POINT('',(0.,0.,0.));
#5196=CARTESIAN_POINT('Origin',(-16.,-116.5,6.07153216591882E-15));
#5197=CARTESIAN_POINT('',(-14.,-116.5,6.07153216591882E-15));
#5198=CARTESIAN_POINT('Origin',(-16.,-116.5,6.07153216591882E-15));
#5199=CARTESIAN_POINT('',(-14.,-116.5,-2.));
#5200=CARTESIAN_POINT('',(-14.,-116.5,6.07153216591882E-15));
#5201=CARTESIAN_POINT('Origin',(-16.,-116.5,-2.));
#5202=CARTESIAN_POINT('Origin',(-19.5,-120.,-2.));
#5203=CARTESIAN_POINT('',(-19.5,-116.5,-2.));
#5204=CARTESIAN_POINT('',(-19.5,-102.858571571457,-2.));
#5205=CARTESIAN_POINT('',(-19.5,-120.,-2.));
#5206=CARTESIAN_POINT('',(-19.5,-116.5,0.));
#5207=CARTESIAN_POINT('',(-19.5,-116.5,-2.));
#5208=CARTESIAN_POINT('',(-19.5,-102.858571571457,0.));
#5209=CARTESIAN_POINT('',(-19.5,-120.,0.));
#5210=CARTESIAN_POINT('',(-19.5,-110.,-0.999999999999999));
#5211=CARTESIAN_POINT('Ctrl Pts',(-19.5,-102.858571571457,-1.05422916773102E-14));
#5212=CARTESIAN_POINT('Ctrl Pts',(-19.5,-105.799159747916,-1.69574446668887E-14));
#5213=CARTESIAN_POINT('Ctrl Pts',(-19.5,-110.,-1.));
#5214=CARTESIAN_POINT('Ctrl Pts',(-19.5,-110.,-0.999999999999976));
#5215=CARTESIAN_POINT('Ctrl Pts',(-19.5,-105.799159747916,-1.99999999999999));
#5216=CARTESIAN_POINT('Ctrl Pts',(-19.5,-102.858571571457,-1.99999999999999));
#5217=CARTESIAN_POINT('Origin',(-12.5,-120.,-2.));
#5218=CARTESIAN_POINT('',(-12.5,-116.5,0.));
#5219=CARTESIAN_POINT('',(-12.5,-73.0000000000001,0.));
#5220=CARTESIAN_POINT('',(-12.5,-120.,0.));
#5221=CARTESIAN_POINT('',(-12.5,-116.5,-2.));
#5222=CARTESIAN_POINT('',(-12.5,-116.5,-2.));
#5223=CARTESIAN_POINT('',(-12.5,-73.0000000000001,-2.));
#5224=CARTESIAN_POINT('',(-12.5,-120.,-2.));
#5225=CARTESIAN_POINT('',(-12.5,-70.,-1.));
#5226=CARTESIAN_POINT('',(-12.5,-80.,-4.3333333333333));
#5227=CARTESIAN_POINT('',(-12.5,-80.,2.3333333333333));
#5228=CARTESIAN_POINT('Origin',(0.,0.,-2.));
#5229=CARTESIAN_POINT('Origin',(-16.,-116.5,-2.));
#5230=CARTESIAN_POINT('',(-19.5,-80.,-2.));
#5231=CARTESIAN_POINT('',(-19.5,0.,-2.));
#5232=CARTESIAN_POINT('Origin',(-12.5,-80.,-2.));
#5233=CARTESIAN_POINT('Origin',(0.,0.,0.));
#5234=CARTESIAN_POINT('Origin',(-16.,-116.5,0.));
#5235=CARTESIAN_POINT('',(-19.5,-80.,0.));
#5236=CARTESIAN_POINT('Origin',(-12.5,-80.,0.));
#5237=CARTESIAN_POINT('',(-19.5,-102.858571571457,0.));
#5238=CARTESIAN_POINT('Origin',(-12.5,-102.858571571457,0.));
#5239=CARTESIAN_POINT('',(-22.5,-102.858571571457,-0.999999999999999));
#5240=CARTESIAN_POINT('Origin',(-12.5,-102.858571571457,-1.));
#5241=CARTESIAN_POINT('',(-22.5,-102.858571571457,-1.));
#5242=CARTESIAN_POINT('Origin',(-22.5,0.,-1.));
#5243=CARTESIAN_POINT('',(-22.5,-80.,-0.999999999999999));
#5244=CARTESIAN_POINT('',(-22.5,-80.,-1.));
#5245=CARTESIAN_POINT('',(-22.5,-80.,-1.));
#5246=CARTESIAN_POINT('Origin',(-12.5,-102.858571571457,-2.));
#5247=CARTESIAN_POINT('',(-19.5,-102.858571571457,-2.));
#5248=CARTESIAN_POINT('Origin',(-12.5,-80.,0.));
#5249=CARTESIAN_POINT('Origin',(-12.5,-80.,-1.));
#5250=CARTESIAN_POINT('Origin',(-22.5,0.,-0.999999999999999));
#5251=CARTESIAN_POINT('',(-19.5,-80.,-2.));
#5252=CARTESIAN_POINT('Origin',(-12.5,-80.,-2.));
#5253=CARTESIAN_POINT('Origin',(-16.,-116.5,-2.));
#5254=CARTESIAN_POINT('',(0.,0.,0.));
#5255=CARTESIAN_POINT('Origin',(-16.,-116.5,-2.00000000000001));
#5256=CARTESIAN_POINT('',(-18.,-116.5,-2.00000000000001));
#5257=CARTESIAN_POINT('Origin',(-16.,-116.5,-2.00000000000001));
#5258=CARTESIAN_POINT('',(-18.,-116.5,-1.30451205393456E-14));
#5259=CARTESIAN_POINT('',(-18.,-116.5,-2.00000000000001));
#5260=CARTESIAN_POINT('Origin',(-16.,-116.5,-1.38777878078145E-14));
#5261=CARTESIAN_POINT('Origin',(-22.5,-105.,-1.50000000000001));
#5262=CARTESIAN_POINT('',(-22.4343957334051,-104.002154280361,-1.00000000000001));
#5263=CARTESIAN_POINT('',(-22.0315240935613,-105.883476273074,-1.00000000000001));
#5264=CARTESIAN_POINT('Ctrl Pts',(-22.4343957334051,-104.002154280361,-1.00000000000001));
#5265=CARTESIAN_POINT('Ctrl Pts',(-22.3711029895888,-104.006315518874,-1.02080054812375));
#5266=CARTESIAN_POINT('Ctrl Pts',(-22.3070770846659,-104.016655879379,-1.04160380896525));
#5267=CARTESIAN_POINT('Ctrl Pts',(-22.1218994092456,-104.065586327466,-1.10093418649023));
#5268=CARTESIAN_POINT('Ctrl Pts',(-22.0050091877668,-104.122719505682,-1.13722283104251));
#5269=CARTESIAN_POINT('Ctrl Pts',(-21.8158438636493,-104.261835149209,-1.19313252973015));
#5270=CARTESIAN_POINT('Ctrl Pts',(-21.7287811554342,-104.351555835029,-1.21730844885347));
#5271=CARTESIAN_POINT('Ctrl Pts',(-21.5941724070256,-104.558712433615,-1.24965683324256));
#5272=CARTESIAN_POINT('Ctrl Pts',(-21.5466705229745,-104.676187630697,-1.25776140553084));
#5273=CARTESIAN_POINT('Ctrl Pts',(-21.4976674225048,-104.905021337286,-1.25776140553084));
#5274=CARTESIAN_POINT('Ctrl Pts',(-21.4928968258581,-105.031647133732,-1.24965683324256));
#5275=CARTESIAN_POINT('Ctrl Pts',(-21.5308692848446,-105.275760762692,-1.21730844885347));
#5276=CARTESIAN_POINT('Ctrl Pts',(-21.5735559693207,-105.393266352322,-1.19313252973015));
#5277=CARTESIAN_POINT('Ctrl Pts',(-21.6891640143735,-105.597647031549,-1.13722283104251));
#5278=CARTESIAN_POINT('Ctrl Pts',(-21.7724073571378,-105.697637380163,-1.10093418649023));
#5279=CARTESIAN_POINT('Ctrl Pts',(-21.9213088988862,-105.818108501553,-1.04160380896526));
#5280=CARTESIAN_POINT('Ctrl Pts',(-21.975485733804,-105.8537611328,-1.02080054812375));
#5281=CARTESIAN_POINT('Ctrl Pts',(-22.0315240935613,-105.883476273074,-1.00000000000001));
#5282=CARTESIAN_POINT('Ctrl Pts',(-22.0315240935613,-105.883476273074,-1.00000000000001));
#5283=CARTESIAN_POINT('Ctrl Pts',(-21.975485733804,-105.8537611328,-0.979199451876273));
#5284=CARTESIAN_POINT('Ctrl Pts',(-21.9213088988862,-105.818108501553,-0.958396191034767));
#5285=CARTESIAN_POINT('Ctrl Pts',(-21.7724073571378,-105.697637380163,-0.899065813509789));
#5286=CARTESIAN_POINT('Ctrl Pts',(-21.6891640143735,-105.597647031549,-0.862777168957508));
#5287=CARTESIAN_POINT('Ctrl Pts',(-21.5735559693207,-105.393266352322,-0.806867470269865));
#5288=CARTESIAN_POINT('Ctrl Pts',(-21.5308692848446,-105.275760762692,-0.782691551146544));
#5289=CARTESIAN_POINT('Ctrl Pts',(-21.4928968258581,-105.031647133732,-0.750343166757458));
#5290=CARTESIAN_POINT('Ctrl Pts',(-21.4976674225048,-104.905021337286,-0.742238594469177));
#5291=CARTESIAN_POINT('Ctrl Pts',(-21.5466705229745,-104.676187630697,-0.742238594469178));
#5292=CARTESIAN_POINT('Ctrl Pts',(-21.5941724070256,-104.558712433615,-0.75034316675746));
#5293=CARTESIAN_POINT('Ctrl Pts',(-21.7287811554342,-104.351555835029,-0.782691551146546));
#5294=CARTESIAN_POINT('Ctrl Pts',(-21.8158438636493,-104.261835149209,-0.806867470269865));
#5295=CARTESIAN_POINT('Ctrl Pts',(-22.0050091877668,-104.122719505682,-0.862777168957507));
#5296=CARTESIAN_POINT('Ctrl Pts',(-22.1218994092456,-104.065586327466,-0.899065813509786));
#5297=CARTESIAN_POINT('Ctrl Pts',(-22.3070770846659,-104.016655879379,-0.958396191034765));
#5298=CARTESIAN_POINT('Ctrl Pts',(-22.3711029895888,-104.006315518874,-0.979199451876272));
#5299=CARTESIAN_POINT('Ctrl Pts',(-22.4343957334051,-104.002154280361,-1.00000000000001));
#5300=CARTESIAN_POINT('Origin',(-22.5,-100.,-1.50000000000001));
#5301=CARTESIAN_POINT('',(-22.5,-99.0000000000013,-1.00000000000001));
#5302=CARTESIAN_POINT('',(-22.5,-100.999999999999,-1.00000000000001));
#5303=CARTESIAN_POINT('Origin',(-22.4999999999999,-100.,-1.00000000000005));
#5304=CARTESIAN_POINT('Origin',(-22.4999999999992,-99.9999999999994,-0.999999999999742));
#5305=CARTESIAN_POINT('Origin',(-22.5,-95.0000000000001,-1.50000000000001));
#5306=CARTESIAN_POINT('',(-22.5,-94.0000000000013,-1.00000000000001));
#5307=CARTESIAN_POINT('',(-22.5,-95.9999999999988,-1.00000000000001));
#5308=CARTESIAN_POINT('Origin',(-22.5000000000019,-95.000000000002,-0.999999999999375));
#5309=CARTESIAN_POINT('Origin',(-22.4999999999992,-94.9999999999993,-0.999999999999733));
#5310=CARTESIAN_POINT('Origin',(-22.5,-90.0000000000001,-1.50000000000001));
#5311=CARTESIAN_POINT('',(-22.5,-89.0000000000013,-1.00000000000001));
#5312=CARTESIAN_POINT('',(-22.5,-90.9999999999988,-1.00000000000001));
#5313=CARTESIAN_POINT('Origin',(-22.5000000000003,-90.0000000000003,-0.999999999999934));
#5314=CARTESIAN_POINT('Origin',(-22.5000000000004,-90.0000000000005,-1.00000000000014));
#5315=CARTESIAN_POINT('Origin',(-22.5,-85.0000000000001,-1.50000000000001));
#5316=CARTESIAN_POINT('',(-22.5,-84.0000000000013,-1.00000000000001));
#5317=CARTESIAN_POINT('',(-22.5,-85.9999999999988,-1.00000000000001));
#5318=CARTESIAN_POINT('Origin',(-22.4999999999998,-85.,-1.00000000000009));
#5319=CARTESIAN_POINT('Origin',(-22.4999999999998,-84.9999999999999,-0.999999999999931));
#5320=CARTESIAN_POINT('Origin',(-22.5,-80.0000000000001,-1.50000000000001));
#5321=CARTESIAN_POINT('',(-22.4500000000001,-79.0012507822294,-1.00000000000001));
#5322=CARTESIAN_POINT('',(-21.5000000000012,-80.,-1.33333333333294));
#5323=CARTESIAN_POINT('Ctrl Pts',(-22.4500000000001,-79.0012507822294,-0.999999999999996));
#5324=CARTESIAN_POINT('Ctrl Pts',(-22.433178965212,-79.0020928872588,-1.00560701159605));
#5325=CARTESIAN_POINT('Ctrl Pts',(-22.4164991934282,-79.003354331563,-1.01118110520576));
#5326=CARTESIAN_POINT('Ctrl Pts',(-22.4000000000002,-79.0050125628946,-1.01670854297789));
#5327=CARTESIAN_POINT('Ctrl Pts',(-22.2827867384775,-79.0167929389226,-1.05597646307129));
#5328=CARTESIAN_POINT('Ctrl Pts',(-22.1591192674472,-79.0513996254551,-1.0981750197407));
#5329=CARTESIAN_POINT('Ctrl Pts',(-21.9333812202348,-79.1663420781321,-1.17665640788624));
#5330=CARTESIAN_POINT('Ctrl Pts',(-21.8313133719646,-79.2467073428857,-1.21290387580589));
#5331=CARTESIAN_POINT('Ctrl Pts',(-21.6759155424808,-79.4222458403709,-1.26875239207065));
#5332=CARTESIAN_POINT('Ctrl Pts',(-21.6097645938577,-79.5280963986251,-1.29290860193093));
#5333=CARTESIAN_POINT('Ctrl Pts',(-21.5217810563411,-79.7585465079784,-1.32523367161175));
#5334=CARTESIAN_POINT('Ctrl Pts',(-21.5000000000012,-79.8831754310448,-1.33333333333292));
#5335=CARTESIAN_POINT('Ctrl Pts',(-21.5000000000012,-80.0000000000001,-1.33333333333292));
#5336=CARTESIAN_POINT('',(-22.5,-80.9999999999988,-1.00000000000001));
#5337=CARTESIAN_POINT('Origin',(-22.4999999999997,-80.0000000000004,-1.00000000000013));
#5338=CARTESIAN_POINT('',(-21.5000000000012,-80.,-0.666666666667091));
#5339=CARTESIAN_POINT('Origin',(-22.4999999999995,-80.0000000000006,-0.999999999999846));
#5340=CARTESIAN_POINT('Ctrl Pts',(-21.5000000000012,-80.0000000000001,-0.666666666667071));
#5341=CARTESIAN_POINT('Ctrl Pts',(-21.5000000000012,-79.8831754310448,-0.666666666667072));
#5342=CARTESIAN_POINT('Ctrl Pts',(-21.5217810563411,-79.7585465079784,-0.67476632838824));
#5343=CARTESIAN_POINT('Ctrl Pts',(-21.6097645938577,-79.5280963986251,-0.707091398069062));
#5344=CARTESIAN_POINT('Ctrl Pts',(-21.6759155424808,-79.4222458403709,-0.731247607929342));
#5345=CARTESIAN_POINT('Ctrl Pts',(-21.8313133719646,-79.2467073428857,-0.787096124194101));
#5346=CARTESIAN_POINT('Ctrl Pts',(-21.9333812202348,-79.1663420781321,-0.823343592113753));
#5347=CARTESIAN_POINT('Ctrl Pts',(-22.1591192674472,-79.0513996254551,-0.901824980259289));
#5348=CARTESIAN_POINT('Ctrl Pts',(-22.2827867384775,-79.0167929389226,-0.944023536928704));
#5349=CARTESIAN_POINT('Ctrl Pts',(-22.4000000000002,-79.0050125628946,-0.983291457022097));
#5350=CARTESIAN_POINT('Ctrl Pts',(-22.4164991934282,-79.003354331563,-0.988818894794232));
#5351=CARTESIAN_POINT('Ctrl Pts',(-22.433178965212,-79.0020928872588,-0.994392988403943));
#5352=CARTESIAN_POINT('Ctrl Pts',(-22.4500000000001,-79.0012507822294,-0.999999999999997));
#5353=CARTESIAN_POINT('Origin',(-16.3268343236508,-70.7612046748876,-1.50000000000001));
#5354=CARTESIAN_POINT('',(-15.3849761916216,-70.4251938727838,-1.00000000000001));
#5355=CARTESIAN_POINT('',(-17.2304241124439,-71.1896034302417,-1.00000000000001));
#5356=CARTESIAN_POINT('Ctrl Pts',(-15.3849761916216,-70.4251938727838,-0.999999999999998));
#5357=CARTESIAN_POINT('Ctrl Pts',(-15.3793170638938,-70.4410567421835,-1.00560701159611));
#5358=CARTESIAN_POINT('Ctrl Pts',(-15.3740994141505,-70.4569495757777,-1.01118110520587));
#5359=CARTESIAN_POINT('Ctrl Pts',(-15.3693174521657,-70.4728274205466,-1.01670854297806));
#5360=CARTESIAN_POINT('Ctrl Pts',(-15.335345527225,-70.5856265085394,-1.0559764630715));
#5361=CARTESIAN_POINT('Ctrl Pts',(-15.3199924443146,-70.7131237594469,-1.09817501974097));
#5362=CARTESIAN_POINT('Ctrl Pts',(-15.3397992130368,-70.9656650932907,-1.17665640788659));
#5363=CARTESIAN_POINT('Ctrl Pts',(-15.3749873617574,-71.090717944594,-1.21290387580629));
#5364=CARTESIAN_POINT('Ctrl Pts',(-15.477695611983,-71.3014624933809,-1.26875239207111));
#5365=CARTESIAN_POINT('Ctrl Pts',(-15.5501739041858,-71.4030852558205,-1.29290860193142));
#5366=CARTESIAN_POINT('Ctrl Pts',(-15.729412201354,-71.5725608841664,-1.32523367161228));
#5367=CARTESIAN_POINT('Ctrl Pts',(-15.8362190631334,-71.6403773803664,-1.33333333333346));
#5368=CARTESIAN_POINT('Ctrl Pts',(-16.0520827194381,-71.7297910344313,-1.33333333333346));
#5369=CARTESIAN_POINT('Ctrl Pts',(-16.1755600800189,-71.7573613863334,-1.32523367161228));
#5370=CARTESIAN_POINT('Ctrl Pts',(-16.4221380614441,-71.7642646356601,-1.29290860193142));
#5371=CARTESIAN_POINT('Ctrl Pts',(-16.5452460977935,-71.7436563831215,-1.26875239207111));
#5372=CARTESIAN_POINT('Ctrl Pts',(-16.7668906975571,-71.6672631837946,-1.21290387580629));
#5373=CARTESIAN_POINT('Ctrl Pts',(-16.8801981952981,-71.6037192432091,-1.1766564078866));
#5374=CARTESIAN_POINT('Ctrl Pts',(-17.0727773854659,-71.4391510539951,-1.09817501974097));
#5375=CARTESIAN_POINT('Ctrl Pts',(-17.1520752871271,-71.3381406142577,-1.0559764630715));
#5376=CARTESIAN_POINT('Ctrl Pts',(-17.2156604826226,-71.2197491462776,-1.01118110520602));
#5377=CARTESIAN_POINT('Ctrl Pts',(-17.2232089775138,-71.204821780356,-1.0056070115964));
#5378=CARTESIAN_POINT('Ctrl Pts',(-17.2304241124433,-71.1896034302429,-1.00000000000044));
#5379=CARTESIAN_POINT('Ctrl Pts',(-17.2304241124439,-71.1896034302417,-1.));
#5380=CARTESIAN_POINT('Ctrl Pts',(-17.2232089775142,-71.2048217803552,-0.994392988403892));
#5381=CARTESIAN_POINT('Ctrl Pts',(-17.2156604826228,-71.2197491462772,-0.988818894794122));
#5382=CARTESIAN_POINT('Ctrl Pts',(-17.1520752871271,-71.3381406142577,-0.944023536928495));
#5383=CARTESIAN_POINT('Ctrl Pts',(-17.0727773854659,-71.4391510539951,-0.901824980259031));
#5384=CARTESIAN_POINT('Ctrl Pts',(-16.8801981952981,-71.6037192432091,-0.823343592113403));
#5385=CARTESIAN_POINT('Ctrl Pts',(-16.7668906975571,-71.6672631837946,-0.787096124193711));
#5386=CARTESIAN_POINT('Ctrl Pts',(-16.5452460977935,-71.7436563831215,-0.731247607928886));
#5387=CARTESIAN_POINT('Ctrl Pts',(-16.4221380614441,-71.7642646356601,-0.707091398068581));
#5388=CARTESIAN_POINT('Ctrl Pts',(-16.1755600800189,-71.7573613863334,-0.674766328387719));
#5389=CARTESIAN_POINT('Ctrl Pts',(-16.0520827194381,-71.7297910344313,-0.666666666666536));
#5390=CARTESIAN_POINT('Ctrl Pts',(-15.8362190631334,-71.6403773803664,-0.666666666666536));
#5391=CARTESIAN_POINT('Ctrl Pts',(-15.729412201354,-71.5725608841664,-0.674766328387716));
#5392=CARTESIAN_POINT('Ctrl Pts',(-15.5501739041858,-71.4030852558205,-0.707091398068578));
#5393=CARTESIAN_POINT('Ctrl Pts',(-15.477695611983,-71.3014624933809,-0.731247607928885));
#5394=CARTESIAN_POINT('Ctrl Pts',(-15.3749873617574,-71.090717944594,-0.78709612419371));
#5395=CARTESIAN_POINT('Ctrl Pts',(-15.3397992130368,-70.9656650932907,-0.823343592113405));
#5396=CARTESIAN_POINT('Ctrl Pts',(-15.3199924443146,-70.7131237594469,-0.901824980259028));
#5397=CARTESIAN_POINT('Ctrl Pts',(-15.335345527225,-70.5856265085394,-0.944023536928495));
#5398=CARTESIAN_POINT('Ctrl Pts',(-15.3693174521657,-70.4728274205466,-0.983291457021933));
#5399=CARTESIAN_POINT('Ctrl Pts',(-15.3740994141504,-70.4569495757781,-0.988818894793977));
#5400=CARTESIAN_POINT('Ctrl Pts',(-15.3793170638935,-70.4410567421843,-0.994392988403597));
#5401=CARTESIAN_POINT('Ctrl Pts',(-15.3849761916211,-70.4251938727851,-0.999999999999556));
#5402=CARTESIAN_POINT('Origin',(-19.5710678118652,-72.9289321881353,-1.50000000000001));
#5403=CARTESIAN_POINT('',(-18.8294901282151,-72.2580651826028,-1.00000000000001));
#5404=CARTESIAN_POINT('',(-20.2419348173977,-73.6705098717854,-1.00000000000001));
#5405=CARTESIAN_POINT('Ctrl Pts',(-18.8294901282151,-72.2580651826028,-0.999999999999999));
#5406=CARTESIAN_POINT('Ctrl Pts',(-18.8181913186264,-72.270554908545,-1.00560701159615));
#5407=CARTESIAN_POINT('Ctrl Pts',(-18.8072889147109,-72.2832412641038,-1.01118110520595));
#5408=CARTESIAN_POINT('Ctrl Pts',(-18.796794769773,-72.2960805022804,-1.01670854297818));
#5409=CARTESIAN_POINT('Ctrl Pts',(-18.7222424614796,-72.3872927781225,-1.05597646307161));
#5410=CARTESIAN_POINT('Ctrl Pts',(-18.6592669768233,-72.4992095082219,-1.09817501974108));
#5411=CARTESIAN_POINT('Ctrl Pts',(-18.5809226606016,-72.740106999912,-1.17665640788671));
#5412=CARTESIAN_POINT('Ctrl Pts',(-18.5655766166277,-72.8691066912443,-1.2129038758064));
#5413=CARTESIAN_POINT('Ctrl Pts',(-18.5798182195492,-73.1031140121853,-1.26875239207123));
#5414=CARTESIAN_POINT('Ctrl Pts',(-18.6078900827299,-73.2247374440727,-1.29290860193154));
#5415=CARTESIAN_POINT('Ctrl Pts',(-18.7086291617681,-73.4499040351326,-1.3252336716124));
#5416=CARTESIAN_POINT('Ctrl Pts',(-18.7813535857611,-73.5534315244043,-1.33333333333357));
#5417=CARTESIAN_POINT('Ctrl Pts',(-18.9465684755962,-73.7186464142394,-1.33333333333357));
#5418=CARTESIAN_POINT('Ctrl Pts',(-19.0500959648678,-73.7913708382324,-1.32523367161239));
#5419=CARTESIAN_POINT('Ctrl Pts',(-19.2752625559277,-73.8921099172706,-1.29290860193153));
#5420=CARTESIAN_POINT('Ctrl Pts',(-19.3968859878151,-73.9201817804513,-1.26875239207122));
#5421=CARTESIAN_POINT('Ctrl Pts',(-19.6308933087562,-73.9344233833728,-1.2129038758064));
#5422=CARTESIAN_POINT('Ctrl Pts',(-19.7598930000884,-73.9190773393989,-1.17665640788671));
#5423=CARTESIAN_POINT('Ctrl Pts',(-20.0007904917785,-73.8407330231772,-1.09817501974108));
#5424=CARTESIAN_POINT('Ctrl Pts',(-20.1127072218779,-73.7777575385209,-1.05597646307161));
#5425=CARTESIAN_POINT('Ctrl Pts',(-20.2167587358963,-73.6927110852899,-1.01118110520609));
#5426=CARTESIAN_POINT('Ctrl Pts',(-20.2294450914547,-73.6818086813747,-1.00560701159644));
#5427=CARTESIAN_POINT('Ctrl Pts',(-20.2419348173967,-73.6705098717863,-1.00000000000044));
#5428=CARTESIAN_POINT('Ctrl Pts',(-20.2419348173977,-73.6705098717854,-0.999999999999999));
#5429=CARTESIAN_POINT('Ctrl Pts',(-20.2294450914554,-73.6818086813741,-0.994392988403851));
#5430=CARTESIAN_POINT('Ctrl Pts',(-20.2167587358967,-73.6927110852896,-0.988818894794047));
#5431=CARTESIAN_POINT('Ctrl Pts',(-20.1127072218779,-73.7777575385209,-0.944023536928382));
#5432=CARTESIAN_POINT('Ctrl Pts',(-20.0007904917785,-73.8407330231772,-0.901824980258916));
#5433=CARTESIAN_POINT('Ctrl Pts',(-19.7598930000884,-73.9190773393989,-0.823343592113289));
#5434=CARTESIAN_POINT('Ctrl Pts',(-19.6308933087562,-73.9344233833728,-0.787096124193595));
#5435=CARTESIAN_POINT('Ctrl Pts',(-19.3968859878151,-73.9201817804513,-0.73124760792877));
#5436=CARTESIAN_POINT('Ctrl Pts',(-19.2752625559277,-73.8921099172706,-0.707091398068464));
#5437=CARTESIAN_POINT('Ctrl Pts',(-19.0500959648678,-73.7913708382324,-0.674766328387601));
#5438=CARTESIAN_POINT('Ctrl Pts',(-18.9465684755962,-73.7186464142394,-0.666666666666421));
#5439=CARTESIAN_POINT('Ctrl Pts',(-18.7813535857611,-73.5534315244043,-0.666666666666421));
#5440=CARTESIAN_POINT('Ctrl Pts',(-18.7086291617681,-73.4499040351326,-0.674766328387602));
#5441=CARTESIAN_POINT('Ctrl Pts',(-18.6078900827299,-73.2247374440727,-0.707091398068464));
#5442=CARTESIAN_POINT('Ctrl Pts',(-18.5798182195492,-73.1031140121853,-0.731247607928769));
#5443=CARTESIAN_POINT('Ctrl Pts',(-18.5655766166277,-72.8691066912443,-0.787096124193594));
#5444=CARTESIAN_POINT('Ctrl Pts',(-18.5809226606016,-72.740106999912,-0.823343592113288));
#5445=CARTESIAN_POINT('Ctrl Pts',(-18.6592669768233,-72.4992095082219,-0.901824980258915));
#5446=CARTESIAN_POINT('Ctrl Pts',(-18.7222424614796,-72.3872927781225,-0.944023536928382));
#5447=CARTESIAN_POINT('Ctrl Pts',(-18.796794769773,-72.2960805022804,-0.98329145702182));
#5448=CARTESIAN_POINT('Ctrl Pts',(-18.8072889147106,-72.2832412641041,-0.9888188947939));
#5449=CARTESIAN_POINT('Ctrl Pts',(-18.8181913186258,-72.2705549085457,-0.994392988403553));
#5450=CARTESIAN_POINT('Ctrl Pts',(-18.8294901282142,-72.2580651826038,-0.99999999999955));
#5451=CARTESIAN_POINT('Origin',(-21.7387953251129,-76.1731656763492,-1.50000000000001));
#5452=CARTESIAN_POINT('',(-21.3103965697588,-75.269575887557,-1.00000000000001));
#5453=CARTESIAN_POINT('',(-22.074806127216,-77.1150238083777,-1.00000000000001));
#5454=CARTESIAN_POINT('Ctrl Pts',(-21.3103965697588,-75.269575887557,-1.));
#5455=CARTESIAN_POINT('Ctrl Pts',(-21.2951782196454,-75.2767910224866,-1.00560701159606));
#5456=CARTESIAN_POINT('Ctrl Pts',(-21.2802508537235,-75.2843395173779,-1.01118110520577));
#5457=CARTESIAN_POINT('Ctrl Pts',(-21.2656421642701,-75.2921854913377,-1.01670854297791));
#5458=CARTESIAN_POINT('Ctrl Pts',(-21.1618593857433,-75.3479247128735,-1.05597646307131));
#5459=CARTESIAN_POINT('Ctrl Pts',(-21.060848946006,-75.4272226145347,-1.09817501974074));
#5460=CARTESIAN_POINT('Ctrl Pts',(-20.8962807567921,-75.6198018047023,-1.17665640788631));
#5461=CARTESIAN_POINT('Ctrl Pts',(-20.8327368162066,-75.7331093024432,-1.21290387580597));
#5462=CARTESIAN_POINT('Ctrl Pts',(-20.7563436168797,-75.9547539022067,-1.26875239207076));
#5463=CARTESIAN_POINT('Ctrl Pts',(-20.7357353643411,-76.077861938556,-1.29290860193104));
#5464=CARTESIAN_POINT('Ctrl Pts',(-20.7426386136678,-76.324439919981,-1.32523367161188));
#5465=CARTESIAN_POINT('Ctrl Pts',(-20.77020896557,-76.4479172805617,-1.33333333333305));
#5466=CARTESIAN_POINT('Ctrl Pts',(-20.8596226196347,-76.6637809368662,-1.33333333333305));
#5467=CARTESIAN_POINT('Ctrl Pts',(-20.9274391158347,-76.7705877986455,-1.32523367161188));
#5468=CARTESIAN_POINT('Ctrl Pts',(-21.0969147441805,-76.9498260958136,-1.29290860193104));
#5469=CARTESIAN_POINT('Ctrl Pts',(-21.1985375066201,-77.0223043880163,-1.26875239207076));
#5470=CARTESIAN_POINT('Ctrl Pts',(-21.4092820554068,-77.1250126382418,-1.21290387580597));
#5471=CARTESIAN_POINT('Ctrl Pts',(-21.5343349067099,-77.1602007869623,-1.17665640788631));
#5472=CARTESIAN_POINT('Ctrl Pts',(-21.7868762405536,-77.1800075556846,-1.09817501974075));
#5473=CARTESIAN_POINT('Ctrl Pts',(-21.914373491461,-77.1646544727742,-1.05597646307131));
#5474=CARTESIAN_POINT('Ctrl Pts',(-22.043050424222,-77.1259005858488,-1.01118110520591));
#5475=CARTESIAN_POINT('Ctrl Pts',(-22.0589432578156,-77.1206829361058,-1.00560701159635));
#5476=CARTESIAN_POINT('Ctrl Pts',(-22.0748061272147,-77.1150238083782,-1.00000000000044));
#5477=CARTESIAN_POINT('Ctrl Pts',(-22.074806127216,-77.1150238083777,-0.999999999999997));
#5478=CARTESIAN_POINT('Ctrl Pts',(-22.0589432578165,-77.1206829361055,-0.994392988403939));
#5479=CARTESIAN_POINT('Ctrl Pts',(-22.0430504242224,-77.1259005858487,-0.988818894794226));
#5480=CARTESIAN_POINT('Ctrl Pts',(-21.914373491461,-77.1646544727742,-0.94402353692868));
#5481=CARTESIAN_POINT('Ctrl Pts',(-21.7868762405536,-77.1800075556846,-0.901824980259249));
#5482=CARTESIAN_POINT('Ctrl Pts',(-21.5343349067099,-77.1602007869623,-0.823343592113684));
#5483=CARTESIAN_POINT('Ctrl Pts',(-21.4092820554068,-77.1250126382418,-0.787096124194018));
#5484=CARTESIAN_POINT('Ctrl Pts',(-21.1985375066201,-77.0223043880163,-0.731247607929237));
#5485=CARTESIAN_POINT('Ctrl Pts',(-21.0969147441805,-76.9498260958136,-0.707091398068949));
#5486=CARTESIAN_POINT('Ctrl Pts',(-20.9274391158347,-76.7705877986455,-0.674766328388114));
#5487=CARTESIAN_POINT('Ctrl Pts',(-20.8596226196347,-76.6637809368662,-0.66666666666694));
#5488=CARTESIAN_POINT('Ctrl Pts',(-20.77020896557,-76.4479172805617,-0.66666666666694));
#5489=CARTESIAN_POINT('Ctrl Pts',(-20.7426386136678,-76.324439919981,-0.674766328388116));
#5490=CARTESIAN_POINT('Ctrl Pts',(-20.7357353643411,-76.0778619385559,-0.707091398068951));
#5491=CARTESIAN_POINT('Ctrl Pts',(-20.7563436168797,-75.9547539022067,-0.731247607929234));
#5492=CARTESIAN_POINT('Ctrl Pts',(-20.8327368162066,-75.7331093024432,-0.787096124194015));
#5493=CARTESIAN_POINT('Ctrl Pts',(-20.8962807567921,-75.6198018047023,-0.823343592113683));
#5494=CARTESIAN_POINT('Ctrl Pts',(-21.060848946006,-75.4272226145347,-0.901824980259247));
#5495=CARTESIAN_POINT('Ctrl Pts',(-21.1618593857433,-75.3479247128735,-0.944023536928678));
#5496=CARTESIAN_POINT('Ctrl Pts',(-21.2656421642701,-75.2921854913377,-0.983291457022086));
#5497=CARTESIAN_POINT('Ctrl Pts',(-21.2802508537231,-75.2843395173782,-0.988818894794077));
#5498=CARTESIAN_POINT('Ctrl Pts',(-21.2951782196446,-75.276791022487,-0.994392988403642));
#5499=CARTESIAN_POINT('Ctrl Pts',(-21.3103965697576,-75.2695758875576,-0.999999999999549));
#5500=CARTESIAN_POINT('Origin',(-19.5,-120.,-2.00000000000001));
#5501=CARTESIAN_POINT('',(-19.5,-116.5,-2.00000000000001));
#5502=CARTESIAN_POINT('',(-19.5,-102.858571571457,-2.00000000000001));
#5503=CARTESIAN_POINT('',(-19.5,-120.,-2.00000000000001));
#5504=CARTESIAN_POINT('',(-19.5,-116.5,-1.38777878078145E-14));
#5505=CARTESIAN_POINT('',(-19.5,-116.5,-2.00000000000001));
#5506=CARTESIAN_POINT('',(-19.5,-102.858571571457,-1.38777878078145E-14));
#5507=CARTESIAN_POINT('',(-19.5,-120.,-1.38777878078145E-14));
#5508=CARTESIAN_POINT('',(-19.5,-110.,-1.00000000000001));
#5509=CARTESIAN_POINT('Ctrl Pts',(-19.5,-102.858571571457,-1.91247983633255E-14));
#5510=CARTESIAN_POINT('Ctrl Pts',(-19.5,-105.799159747916,-2.57409313859276E-14));
#5511=CARTESIAN_POINT('Ctrl Pts',(-19.5,-110.,-0.999999999999999));
#5512=CARTESIAN_POINT('Ctrl Pts',(-19.5,-110.,-0.999999999999988));
#5513=CARTESIAN_POINT('Ctrl Pts',(-19.5,-105.799159747916,-2.));
#5514=CARTESIAN_POINT('Ctrl Pts',(-19.5,-102.858571571457,-2.));
#5515=CARTESIAN_POINT('Origin',(-12.5,-120.,-2.00000000000001));
#5516=CARTESIAN_POINT('',(-12.5,-116.5,-1.38777878078145E-14));
#5517=CARTESIAN_POINT('',(-12.5,-73.0000000000001,0.));
#5518=CARTESIAN_POINT('',(-12.5,-120.,-1.38777878078145E-14));
#5519=CARTESIAN_POINT('',(-12.5,-116.5,-2.00000000000001));
#5520=CARTESIAN_POINT('',(-12.5,-116.5,-2.00000000000001));
#5521=CARTESIAN_POINT('',(-12.5,-73.0000000000001,-2.));
#5522=CARTESIAN_POINT('',(-12.5,-120.,-2.00000000000001));
#5523=CARTESIAN_POINT('',(-12.5,-71.0000000000001,-1.33333333333334));
#5524=CARTESIAN_POINT('',(-12.5,-80.,-4.3333333333333));
#5525=CARTESIAN_POINT('',(-12.5,-71.0000000000001,-0.66666666666667));
#5526=CARTESIAN_POINT('',(-12.5,-71.0000000000001,-1.50000000000001));
#5527=CARTESIAN_POINT('',(-12.5,-80.,2.3333333333333));
#5528=CARTESIAN_POINT('Origin',(0.,-5.55111146474324E-17,-2.));
#5529=CARTESIAN_POINT('Origin',(-16.,-116.5,-2.00000000000001));
#5530=CARTESIAN_POINT('',(-19.5,-80.,-2.00000000000001));
#5531=CARTESIAN_POINT('',(-19.5,-1.40859542590934E-15,-2.00000000000001));
#5532=CARTESIAN_POINT('Origin',(-12.5,-80.,-2.));
#5533=CARTESIAN_POINT('Origin',(0.,0.,0.));
#5534=CARTESIAN_POINT('Origin',(-16.,-116.5,-1.38777878078145E-14));
#5535=CARTESIAN_POINT('',(-19.5,-80.,-1.38777878078145E-14));
#5536=CARTESIAN_POINT('Origin',(-12.5,-80.,0.));
#5537=CARTESIAN_POINT('',(-19.5,-102.858571571457,-1.38777878078145E-14));
#5538=CARTESIAN_POINT('Origin',(-12.5,-102.858571571457,-1.38777878078145E-14));
#5539=CARTESIAN_POINT('Origin',(-12.5,-102.858571571457,-1.00000000000001));
#5540=CARTESIAN_POINT('',(-22.5,-102.858571571457,-1.00000000000001));
#5541=CARTESIAN_POINT('',(-22.5,-102.858571571457,-1.00000000000001));
#5542=CARTESIAN_POINT('Origin',(-12.5,-102.858571571457,-1.00000000000001));
#5543=CARTESIAN_POINT('Origin',(-22.5,-1.58900668570284E-15,-1.00000000000001));
#5544=CARTESIAN_POINT('',(-22.5,-80.,-1.00000000000001));
#5545=CARTESIAN_POINT('',(-22.5,-80.,-1.00000000000001));
#5546=CARTESIAN_POINT('',(-22.5,-80.,-1.00000000000001));
#5547=CARTESIAN_POINT('',(-22.5,-80.,-1.00000000000001));
#5548=CARTESIAN_POINT('',(-22.5,-80.,-1.00000000000001));
#5549=CARTESIAN_POINT('',(-22.5,-80.,-1.00000000000001));
#5550=CARTESIAN_POINT('Origin',(-12.5,-102.858571571457,-2.00000000000001));
#5551=CARTESIAN_POINT('',(-19.5,-102.858571571457,-2.00000000000001));
#5552=CARTESIAN_POINT('Origin',(-12.5,-80.,0.));
#5553=CARTESIAN_POINT('',(-13.4987492177719,-70.05,-1.00000000000001));
#5554=CARTESIAN_POINT('Ctrl Pts',(-13.4987492177719,-70.05,-1.));
#5555=CARTESIAN_POINT('Ctrl Pts',(-13.4979071127425,-70.0668210347882,-0.994392988403934));
#5556=CARTESIAN_POINT('Ctrl Pts',(-13.4966456684383,-70.083500806572,-0.988818894794213));
#5557=CARTESIAN_POINT('Ctrl Pts',(-13.4832070610786,-70.2172132615229,-0.944023536928626));
#5558=CARTESIAN_POINT('Ctrl Pts',(-13.4486003745461,-70.3408807325533,-0.90182498025916));
#5559=CARTESIAN_POINT('Ctrl Pts',(-13.333657921869,-70.5666187797661,-0.823343592113535));
#5560=CARTESIAN_POINT('Ctrl Pts',(-13.2532926571153,-70.6686866280364,-0.78709612419384));
#5561=CARTESIAN_POINT('Ctrl Pts',(-13.0777541596298,-70.8240844575203,-0.731247607929015));
#5562=CARTESIAN_POINT('Ctrl Pts',(-12.9719036013755,-70.8902354061435,-0.707091398068708));
#5563=CARTESIAN_POINT('Ctrl Pts',(-12.7414534920219,-70.9782189436602,-0.674766328387846));
#5564=CARTESIAN_POINT('Ctrl Pts',(-12.6168245689554,-71.0000000000001,-0.666666666666663));
#5565=CARTESIAN_POINT('Ctrl Pts',(-12.5,-71.0000000000001,-0.666666666666664));
#5566=CARTESIAN_POINT('Origin',(-12.5,-80.,-1.00000000000001));
#5567=CARTESIAN_POINT('Origin',(-12.5,-80.,-1.00000000000001));
#5568=CARTESIAN_POINT('Origin',(-12.5,-80.,-1.00000000000001));
#5569=CARTESIAN_POINT('Origin',(-12.5,-80.,-1.00000000000001));
#5570=CARTESIAN_POINT('Origin',(-22.5,-1.58900668570284E-15,-1.00000000000001));
#5571=CARTESIAN_POINT('',(-19.5,-80.,-2.00000000000001));
#5572=CARTESIAN_POINT('Origin',(-12.5,-80.,-2.));
#5573=CARTESIAN_POINT('Ctrl Pts',(-12.5,-71.0000000000001,-1.33333333333334));
#5574=CARTESIAN_POINT('Ctrl Pts',(-12.6168245689554,-71.0000000000001,-1.33333333333334));
#5575=CARTESIAN_POINT('Ctrl Pts',(-12.7414534920219,-70.9782189436602,-1.32523367161216));
#5576=CARTESIAN_POINT('Ctrl Pts',(-12.9719036013755,-70.8902354061435,-1.29290860193129));
#5577=CARTESIAN_POINT('Ctrl Pts',(-13.0777541596298,-70.8240844575203,-1.26875239207099));
#5578=CARTESIAN_POINT('Ctrl Pts',(-13.2532926571153,-70.6686866280364,-1.21290387580616));
#5579=CARTESIAN_POINT('Ctrl Pts',(-13.333657921869,-70.5666187797661,-1.17665640788646));
#5580=CARTESIAN_POINT('Ctrl Pts',(-13.4486003745461,-70.3408807325533,-1.09817501974084));
#5581=CARTESIAN_POINT('Ctrl Pts',(-13.4832070610786,-70.2172132615229,-1.05597646307137));
#5582=CARTESIAN_POINT('Ctrl Pts',(-13.4966456684383,-70.083500806572,-1.01118110520579));
#5583=CARTESIAN_POINT('Ctrl Pts',(-13.4979071127425,-70.0668210347882,-1.00560701159606));
#5584=CARTESIAN_POINT('Ctrl Pts',(-13.4987492177719,-70.05,-0.999999999999998));
#5585=CARTESIAN_POINT('Origin',(-12.5,-70.,-1.50000000000001));
#5586=CARTESIAN_POINT('Origin',(-16.,-116.5,-2.00000000000001));
#5587=CARTESIAN_POINT('',(0.,0.,0.));
#5588=CARTESIAN_POINT('Origin',(-16.,-116.5,0.));
#5589=CARTESIAN_POINT('',(-14.,-116.5,0.));
#5590=CARTESIAN_POINT('Origin',(-16.,-116.5,0.));
#5591=CARTESIAN_POINT('',(-14.,-116.5,-2.));
#5592=CARTESIAN_POINT('',(-14.,-116.5,0.));
#5593=CARTESIAN_POINT('Origin',(-16.,-116.5,-2.));
#5594=CARTESIAN_POINT('Origin',(-16.,-60.,-1.));
#5595=CARTESIAN_POINT('',(-16.,-110.,-2.));
#5596=CARTESIAN_POINT('',(-16.5,-110.,-1.86602540378444));
#5597=CARTESIAN_POINT('Origin',(-16.,-110.,-1.));
#5598=CARTESIAN_POINT('',(-16.5,-110.,-0.133974596215562));
#5599=CARTESIAN_POINT('Origin',(-16.,-110.,-1.));
#5600=CARTESIAN_POINT('',(-16.,-110.,-2.16840434497101E-16));
#5601=CARTESIAN_POINT('Origin',(-16.,-110.,-1.));
#5602=CARTESIAN_POINT('',(-16.,-65.,-2.16840434497101E-16));
#5603=CARTESIAN_POINT('',(-16.,-60.,0.));
#5604=CARTESIAN_POINT('',(-16.8660254037844,-65.,-0.499999999999999));
#5605=CARTESIAN_POINT('Origin',(-16.,-65.,-1.));
#5606=CARTESIAN_POINT('',(-16.8660254037844,-65.,-1.5));
#5607=CARTESIAN_POINT('Origin',(-16.,-65.,-1.));
#5608=CARTESIAN_POINT('',(-16.,-65.,-2.));
#5609=CARTESIAN_POINT('Origin',(-16.,-65.,-1.));
#5610=CARTESIAN_POINT('',(-15.1339745962156,-65.,-1.5));
#5611=CARTESIAN_POINT('Origin',(-16.,-65.,-1.));
#5612=CARTESIAN_POINT('',(-15.1339745962156,-65.,-0.500000000000001));
#5613=CARTESIAN_POINT('Origin',(-16.,-65.,-1.));
#5614=CARTESIAN_POINT('Origin',(-16.,-65.,-1.));
#5615=CARTESIAN_POINT('',(-15.5,-110.,-0.133974596215562));
#5616=CARTESIAN_POINT('Origin',(-16.,-110.,-1.));
#5617=CARTESIAN_POINT('',(-15.5,-110.,-1.86602540378444));
#5618=CARTESIAN_POINT('Origin',(-16.,-110.,-1.));
#5619=CARTESIAN_POINT('Origin',(-16.,-110.,-1.));
#5620=CARTESIAN_POINT('Origin',(-19.5,-110.,-2.));
#5621=CARTESIAN_POINT('',(-16.5,-110.,-2.));
#5622=CARTESIAN_POINT('',(-19.5,-110.,-2.));
#5623=CARTESIAN_POINT('',(-16.5,-110.,-2.));
#5624=CARTESIAN_POINT('Origin',(-19.5,-110.,-2.));
#5625=CARTESIAN_POINT('',(-15.5,-110.,0.));
#5626=CARTESIAN_POINT('',(-19.5,-110.,0.));
#5627=CARTESIAN_POINT('',(-15.5,-110.,-2.));
#5628=CARTESIAN_POINT('Origin',(-19.5,-110.,-2.));
#5629=CARTESIAN_POINT('',(-15.5,-110.,-2.));
#5630=CARTESIAN_POINT('',(-15.5,-110.,-2.));
#5631=CARTESIAN_POINT('',(-19.5,-110.,-2.));
#5632=CARTESIAN_POINT('Origin',(-12.5,-120.,-2.));
#5633=CARTESIAN_POINT('',(-12.5,-116.5,0.));
#5634=CARTESIAN_POINT('',(-12.5,-113.,0.));
#5635=CARTESIAN_POINT('',(-12.5,-120.,0.));
#5636=CARTESIAN_POINT('',(-12.5,-116.5,-2.));
#5637=CARTESIAN_POINT('',(-12.5,-116.5,-2.));
#5638=CARTESIAN_POINT('',(-12.5,-113.,-2.));
#5639=CARTESIAN_POINT('',(-12.5,-120.,-2.));
#5640=CARTESIAN_POINT('',(-12.5,-113.,-1.86602540378444));
#5641=CARTESIAN_POINT('',(-12.5,-113.,0.));
#5642=CARTESIAN_POINT('',(-12.5,-113.,-0.133974596215562));
#5643=CARTESIAN_POINT('Ctrl Pts',(-12.5,-113.,-1.86602540378444));
#5644=CARTESIAN_POINT('Ctrl Pts',(-12.5,-112.999999994851,-1.79379309056833));
#5645=CARTESIAN_POINT('Ctrl Pts',(-12.5,-112.998016056892,-1.72157261890518));
#5646=CARTESIAN_POINT('Ctrl Pts',(-12.5,-112.994568071517,-1.64935667749771));
#5647=CARTESIAN_POINT('Ctrl Pts',(-12.5,-112.991126955866,-1.57728461823149));
#5648=CARTESIAN_POINT('Ctrl Pts',(-12.5,-112.986202428167,-1.50521647175664));
#5649=CARTESIAN_POINT('Ctrl Pts',(-12.5,-112.980844807336,-1.43315321107699));
#5650=CARTESIAN_POINT('Ctrl Pts',(-12.5000000000001,-112.975456373403,-1.36067549543516));
#5651=CARTESIAN_POINT('Ctrl Pts',(-12.5000000000004,-112.969634380623,-1.2881978867471));
#5652=CARTESIAN_POINT('Ctrl Pts',(-12.5000000000009,-112.965223416194,-1.21571467716329));
#5653=CARTESIAN_POINT('Ctrl Pts',(-12.5000000000015,-112.960854143347,-1.14391656485544));
#5654=CARTESIAN_POINT('Ctrl Pts',(-12.5000000000017,-112.958046019663,-1.07211583423837));
#5655=CARTESIAN_POINT('Ctrl Pts',(-12.5000000000009,-112.958037668447,-1.00029810032904));
#5656=CARTESIAN_POINT('Ctrl Pts',(-12.5,-112.958029230024,-0.92773041848443));
#5657=CARTESIAN_POINT('Ctrl Pts',(-12.5000000000001,-112.960891052438,-0.855145461004138));
#5658=CARTESIAN_POINT('Ctrl Pts',(-12.5,-112.965330779693,-0.782557921391285));
#5659=CARTESIAN_POINT('Ctrl Pts',(-12.5,-112.969720668615,-0.710785216057982));
#5660=CARTESIAN_POINT('Ctrl Pts',(-12.5,-112.975478101497,-0.639007098038739));
#5661=CARTESIAN_POINT('Ctrl Pts',(-12.5000000000001,-112.980816251273,-0.56722901058433));
#5662=CARTESIAN_POINT('Ctrl Pts',(-12.5000000000001,-112.986204004162,-0.494783947355154));
#5663=CARTESIAN_POINT('Ctrl Pts',(-12.5000000000001,-112.991153168568,-0.422363403854905));
#5664=CARTESIAN_POINT('Ctrl Pts',(-12.5,-112.994603577269,-0.349890285232024));
#5665=CARTESIAN_POINT('Ctrl Pts',(-12.5,-112.998029264397,-0.277936423787971));
#5666=CARTESIAN_POINT('Ctrl Pts',(-12.5,-112.99999999514,-0.206001183885444));
#5667=CARTESIAN_POINT('Ctrl Pts',(-12.5,-113.,-0.133974596215563));
#5668=CARTESIAN_POINT('',(-12.5,-113.,0.));
#5669=CARTESIAN_POINT('Origin',(-19.5,-120.,-2.));
#5670=CARTESIAN_POINT('',(-19.5,-116.5,-2.));
#5671=CARTESIAN_POINT('',(-19.5,-113.,-2.));
#5672=CARTESIAN_POINT('',(-19.5,-120.,-2.));
#5673=CARTESIAN_POINT('',(-19.5,-116.5,0.));
#5674=CARTESIAN_POINT('',(-19.5,-116.5,-2.));
#5675=CARTESIAN_POINT('',(-19.5,-113.,0.));
#5676=CARTESIAN_POINT('',(-19.5,-120.,0.));
#5677=CARTESIAN_POINT('',(-19.5,-113.,-0.133974596215562));
#5678=CARTESIAN_POINT('',(-19.5,-113.,-2.));
#5679=CARTESIAN_POINT('',(-19.5,-113.,-1.86602540378444));
#5680=CARTESIAN_POINT('Ctrl Pts',(-19.5,-113.,-0.133974596215562));
#5681=CARTESIAN_POINT('Ctrl Pts',(-19.5,-112.999999994851,-0.206206909431671));
#5682=CARTESIAN_POINT('Ctrl Pts',(-19.5,-112.998016056892,-0.278427381094817));
#5683=CARTESIAN_POINT('Ctrl Pts',(-19.5,-112.994568071517,-0.350643322502292));
#5684=CARTESIAN_POINT('Ctrl Pts',(-19.5,-112.991126955866,-0.422715381768518));
#5685=CARTESIAN_POINT('Ctrl Pts',(-19.5,-112.986202428167,-0.494783528243354));
#5686=CARTESIAN_POINT('Ctrl Pts',(-19.5,-112.980844807336,-0.566846788923014));
#5687=CARTESIAN_POINT('Ctrl Pts',(-19.5,-112.975456373403,-0.639324504564845));
#5688=CARTESIAN_POINT('Ctrl Pts',(-19.4999999999997,-112.969634380623,-0.711802113252911));
#5689=CARTESIAN_POINT('Ctrl Pts',(-19.4999999999991,-112.965223416194,-0.784285322836707));
#5690=CARTESIAN_POINT('Ctrl Pts',(-19.4999999999986,-112.960854143347,-0.856083435144543));
#5691=CARTESIAN_POINT('Ctrl Pts',(-19.4999999999983,-112.958046019663,-0.927884165761635));
#5692=CARTESIAN_POINT('Ctrl Pts',(-19.4999999999992,-112.958037668447,-0.999701899670956));
#5693=CARTESIAN_POINT('Ctrl Pts',(-19.5,-112.958029230024,-1.07226958151557));
#5694=CARTESIAN_POINT('Ctrl Pts',(-19.5,-112.960891052438,-1.14485453899585));
#5695=CARTESIAN_POINT('Ctrl Pts',(-19.5,-112.965330779693,-1.21744207860871));
#5696=CARTESIAN_POINT('Ctrl Pts',(-19.5,-112.969720668615,-1.28921478394202));
#5697=CARTESIAN_POINT('Ctrl Pts',(-19.5,-112.975478101497,-1.36099290196126));
#5698=CARTESIAN_POINT('Ctrl Pts',(-19.5,-112.980816251273,-1.43277098941567));
#5699=CARTESIAN_POINT('Ctrl Pts',(-19.4999999999999,-112.986204004162,-1.50521605264485));
#5700=CARTESIAN_POINT('Ctrl Pts',(-19.5,-112.991153168568,-1.5776365961451));
#5701=CARTESIAN_POINT('Ctrl Pts',(-19.5,-112.994603577269,-1.65010971476797));
#5702=CARTESIAN_POINT('Ctrl Pts',(-19.5,-112.998029264397,-1.72206357621201));
#5703=CARTESIAN_POINT('Ctrl Pts',(-19.5,-112.99999999514,-1.79399881611456));
#5704=CARTESIAN_POINT('Ctrl Pts',(-19.5,-113.,-1.86602540378443));
#5705=CARTESIAN_POINT('',(-19.5,-113.,-2.));
#5706=CARTESIAN_POINT('Origin',(-19.5,-110.,-2.));
#5707=CARTESIAN_POINT('',(-16.5,-110.,0.));
#5708=CARTESIAN_POINT('',(-16.5,-110.,-2.));
#5709=CARTESIAN_POINT('',(-19.5,-110.,0.));
#5710=CARTESIAN_POINT('Origin',(0.,0.,-2.));
#5711=CARTESIAN_POINT('Origin',(-16.,-116.5,-2.));
#5712=CARTESIAN_POINT('Origin',(-16.5,-113.,-2.));
#5713=CARTESIAN_POINT('Origin',(-15.5,-113.,-2.));
#5714=CARTESIAN_POINT('Origin',(0.,0.,0.));
#5715=CARTESIAN_POINT('Origin',(-16.,-116.5,0.));
#5716=CARTESIAN_POINT('Origin',(-15.5,-113.,0.));
#5717=CARTESIAN_POINT('Origin',(-16.5,-113.,0.));
#5718=CARTESIAN_POINT('Origin',(-15.4226497308104,-65.,-2.98155597433514E-16));
#5719=CARTESIAN_POINT('',(-15.4226497308104,-65.,-2.98155597433514E-16));
#5720=CARTESIAN_POINT('',(-15.4226497308104,-65.,-2.98155597433514E-16));
#5721=CARTESIAN_POINT('',(-14.8452994616208,-65.,-0.999999999999999));
#5722=CARTESIAN_POINT('',(-15.4226497308104,-65.,-2.98155597433514E-16));
#5723=CARTESIAN_POINT('',(-14.8452994616208,-60.,-0.999999999999999));
#5724=CARTESIAN_POINT('',(-14.8452994616208,-65.,-0.999999999999999));
#5725=CARTESIAN_POINT('',(-15.4226497308104,-60.,-2.98155597433514E-16));
#5726=CARTESIAN_POINT('',(-15.4226497308104,-60.,-2.98155597433514E-16));
#5727=CARTESIAN_POINT('',(-15.4226497308104,-65.,-2.98155597433514E-16));
#5728=CARTESIAN_POINT('Origin',(-16.5773502691896,-65.,-1.35525271560688E-17));
#5729=CARTESIAN_POINT('',(-16.5773502691896,-65.,-1.35525271560688E-17));
#5730=CARTESIAN_POINT('',(-16.5773502691896,-65.,-1.35525271560688E-17));
#5731=CARTESIAN_POINT('',(-16.5773502691896,-65.,-1.35525271560688E-17));
#5732=CARTESIAN_POINT('',(-16.5773502691896,-60.,-1.35525271560688E-17));
#5733=CARTESIAN_POINT('',(-16.5773502691896,-60.,-1.35525271560688E-17));
#5734=CARTESIAN_POINT('',(-16.5773502691896,-65.,-1.35525271560688E-17));
#5735=CARTESIAN_POINT('Origin',(-17.1547005383793,-65.,-0.999999999999997));
#5736=CARTESIAN_POINT('',(-17.1547005383793,-65.,-0.999999999999997));
#5737=CARTESIAN_POINT('',(-17.1547005383793,-65.,-0.999999999999997));
#5738=CARTESIAN_POINT('',(-17.1547005383793,-65.,-0.999999999999997));
#5739=CARTESIAN_POINT('',(-17.1547005383793,-60.,-0.999999999999997));
#5740=CARTESIAN_POINT('',(-17.1547005383793,-60.,-0.999999999999997));
#5741=CARTESIAN_POINT('',(-17.1547005383793,-65.,-0.999999999999997));
#5742=CARTESIAN_POINT('Origin',(-16.5773502691896,-65.,-2.));
#5743=CARTESIAN_POINT('',(-16.5773502691896,-65.,-2.));
#5744=CARTESIAN_POINT('',(-16.5773502691896,-65.,-2.));
#5745=CARTESIAN_POINT('',(-16.5773502691896,-65.,-2.));
#5746=CARTESIAN_POINT('',(-16.5773502691896,-60.,-2.));
#5747=CARTESIAN_POINT('',(-16.5773502691896,-60.,-2.));
#5748=CARTESIAN_POINT('',(-16.5773502691896,-65.,-2.));
#5749=CARTESIAN_POINT('Origin',(-15.4226497308104,-65.,-2.));
#5750=CARTESIAN_POINT('',(-15.4226497308104,-65.,-2.));
#5751=CARTESIAN_POINT('',(-15.4226497308104,-65.,-2.));
#5752=CARTESIAN_POINT('',(-15.4226497308104,-65.,-2.));
#5753=CARTESIAN_POINT('',(-15.4226497308104,-60.,-2.));
#5754=CARTESIAN_POINT('',(-15.4226497308104,-60.,-2.));
#5755=CARTESIAN_POINT('',(-15.4226497308104,-65.,-2.));
#5756=CARTESIAN_POINT('Origin',(-14.8452994616208,-65.,-0.999999999999999));
#5757=CARTESIAN_POINT('',(-14.8452994616208,-65.,-0.999999999999999));
#5758=CARTESIAN_POINT('',(-14.8452994616208,-65.,-0.999999999999999));
#5759=CARTESIAN_POINT('',(-14.8452994616208,-60.,-0.999999999999999));
#5760=CARTESIAN_POINT('Origin',(0.,-65.,0.));
#5761=CARTESIAN_POINT('Origin',(0.,-65.,0.));
#5762=CARTESIAN_POINT('Origin',(0.,-65.,0.));
#5763=CARTESIAN_POINT('Origin',(0.,-65.,0.));
#5764=CARTESIAN_POINT('Origin',(0.,-65.,0.));
#5765=CARTESIAN_POINT('Origin',(0.,-65.,0.));
#5766=CARTESIAN_POINT('Origin',(-16.,-60.,-1.));
#5767=CARTESIAN_POINT('Origin',(-15.5,-113.,-2.));
#5768=CARTESIAN_POINT('Origin',(-15.5,-113.,-0.133974596215562));
#5769=CARTESIAN_POINT('Ctrl Pts',(-12.5,-112.998321408359,-0.0215171208906509));
#5770=CARTESIAN_POINT('Ctrl Pts',(-12.5,-109.953990021186,-0.110365484977496));
#5771=CARTESIAN_POINT('Ctrl Pts',(-15.5454993396585,-110.000007198492,-0.108919528903676));
#5772=CARTESIAN_POINT('Ctrl Pts',(-12.5,-113.001650865752,-0.130615518141873));
#5773=CARTESIAN_POINT('Ctrl Pts',(-12.5,-109.994846910505,-0.129517847817374));
#5774=CARTESIAN_POINT('Ctrl Pts',(-15.5052244365464,-110.000000774232,-0.130950785426593));
#5775=CARTESIAN_POINT('Ctrl Pts',(-12.5,-112.999829763877,-0.240121651459518));
#5776=CARTESIAN_POINT('Ctrl Pts',(-12.5,-110.044590565554,-0.157043650297362));
#5777=CARTESIAN_POINT('Ctrl Pts',(-15.4555037853853,-109.999992849754,-0.157582174193049));
#5778=CARTESIAN_POINT('Ctrl Pts',(-12.5,-112.991171615148,-0.421989183009334));
#5779=CARTESIAN_POINT('Ctrl Pts',(-12.5,-110.144230037263,-0.248024746671439));
#5780=CARTESIAN_POINT('Ctrl Pts',(-15.3483339572922,-109.999976541827,-0.239998260254286));
#5781=CARTESIAN_POINT('Ctrl Pts',(-12.5,-112.986249389692,-0.494130629734298));
#5782=CARTESIAN_POINT('Ctrl Pts',(-12.5,-110.187949454441,-0.295175701491007));
#5783=CARTESIAN_POINT('Ctrl Pts',(-15.299011567492,-109.999969217678,-0.282541606351056));
#5784=CARTESIAN_POINT('Ctrl Pts',(-12.5,-112.975531858613,-0.638340025483971));
#5785=CARTESIAN_POINT('Ctrl Pts',(-12.5,-110.278138535025,-0.42781535733713));
#5786=CARTESIAN_POINT('Ctrl Pts',(-15.1911611365941,-109.999953678584,-0.406847658471516));
#5787=CARTESIAN_POINT('Ctrl Pts',(-12.5,-112.969742052832,-0.710437616206344));
#5788=CARTESIAN_POINT('Ctrl Pts',(-12.5,-110.324934754411,-0.513809199029964));
#5789=CARTESIAN_POINT('Ctrl Pts',(-15.1317804589651,-109.999945443368,-0.489955254864159));
#5790=CARTESIAN_POINT('Ctrl Pts',(-12.5,-112.960920191473,-0.854678268466455));
#5791=CARTESIAN_POINT('Ctrl Pts',(-12.5,-110.397592333861,-0.731264401632342));
#5792=CARTESIAN_POINT('Ctrl Pts',(-15.0350207661438,-109.999932251101,-0.712428738528866));
#5793=CARTESIAN_POINT('Ctrl Pts',(-12.5,-112.95806404802,-0.926824230509072));
#5794=CARTESIAN_POINT('Ctrl Pts',(-12.5000000000005,-110.422001594761,-0.864088334522592));
#5795=CARTESIAN_POINT('Ctrl Pts',(-15.0007136147036,-109.999927765103,-0.853647804036836));
#5796=CARTESIAN_POINT('Ctrl Pts',(-12.5,-112.958016061818,-1.07120954970003));
#5797=CARTESIAN_POINT('Ctrl Pts',(-12.4999999999996,-110.422406145868,-1.13224899582074));
#5798=CARTESIAN_POINT('Ctrl Pts',(-15.0001457739159,-109.999927689389,-1.14241971794702));
#5799=CARTESIAN_POINT('Ctrl Pts',(-12.5,-112.960828724944,-1.14344898114294));
#5800=CARTESIAN_POINT('Ctrl Pts',(-12.4999999999999,-110.398355492936,-1.26557410071784));
#5801=CARTESIAN_POINT('Ctrl Pts',(-15.0339698860841,-109.999932110923,-1.28425554920314));
#5802=CARTESIAN_POINT('Ctrl Pts',(-12.5,-112.969622749834,-1.28798009071552));
#5803=CARTESIAN_POINT('Ctrl Pts',(-12.5000000000001,-110.325910420761,-1.48413970176802));
#5804=CARTESIAN_POINT('Ctrl Pts',(-15.1305184541349,-109.999945269335,-1.50802137948635));
#5805=CARTESIAN_POINT('Ctrl Pts',(-12.5,-112.97542425227,-1.36026880325738));
#5806=CARTESIAN_POINT('Ctrl Pts',(-12.5,-110.279014567801,-1.57069480005754));
#5807=CARTESIAN_POINT('Ctrl Pts',(-15.1900769619304,-109.999953525122,-1.5917262456063));
#5808=CARTESIAN_POINT('Ctrl Pts',(-12.5,-112.986176452745,-1.50483219996039));
#5809=CARTESIAN_POINT('Ctrl Pts',(-12.5,-110.188587950114,-1.70408671874064));
#5810=CARTESIAN_POINT('Ctrl Pts',(-15.2982789162811,-109.999969109764,-1.71678752331027));
#5811=CARTESIAN_POINT('Ctrl Pts',(-12.5,-112.991118555997,-1.57710674240752));
#5812=CARTESIAN_POINT('Ctrl Pts',(-12.4999999999996,-110.144750106835,-1.75144466546231));
#5813=CARTESIAN_POINT('Ctrl Pts',(-15.3477573301302,-109.999976455226,-1.75952009740825));
#5814=CARTESIAN_POINT('Ctrl Pts',(-12.5,-112.999819986014,-1.75935530906393));
#5815=CARTESIAN_POINT('Ctrl Pts',(-12.5000000000006,-110.044829996224,-1.84282328506315));
#5816=CARTESIAN_POINT('Ctrl Pts',(-15.455261801624,-109.999992811267,-1.84228939912907));
#5817=CARTESIAN_POINT('Ctrl Pts',(-12.5,-113.001670882596,-1.86929829726474));
#5818=CARTESIAN_POINT('Ctrl Pts',(-12.5000000000052,-109.994838487951,-1.87052042344478));
#5819=CARTESIAN_POINT('Ctrl Pts',(-15.5052368990814,-110.000000775553,-1.86906791930568));
#5820=CARTESIAN_POINT('Ctrl Pts',(-12.5,-112.998303161317,-1.97915370173891));
#5821=CARTESIAN_POINT('Ctrl Pts',(-12.4999999999913,-109.953739602693,-1.88974229707348));
#5822=CARTESIAN_POINT('Ctrl Pts',(-15.5457412933844,-110.000007237571,-1.89120504794152));
#5823=CARTESIAN_POINT('Origin',(-15.5,-113.,-1.86602540378444));
#5824=CARTESIAN_POINT('Origin',(-15.5,-113.,-2.));
#5825=CARTESIAN_POINT('Origin',(-16.5,-113.,-2.));
#5826=CARTESIAN_POINT('Origin',(-16.5,-113.,-0.133974596215562));
#5827=CARTESIAN_POINT('Ctrl Pts',(-19.5,-112.998321408359,-1.97848287910703));
#5828=CARTESIAN_POINT('Ctrl Pts',(-19.5,-109.953990021188,-1.88963451502302));
#5829=CARTESIAN_POINT('Ctrl Pts',(-16.4545006603424,-110.000007198492,-1.89108047109586));
#5830=CARTESIAN_POINT('Ctrl Pts',(-19.5,-113.001650865752,-1.86938448185662));
#5831=CARTESIAN_POINT('Ctrl Pts',(-19.5,-109.994846910506,-1.87048215218166));
#5832=CARTESIAN_POINT('Ctrl Pts',(-16.4947755634543,-110.000000774232,-1.86904921457304));
#5833=CARTESIAN_POINT('Ctrl Pts',(-19.5,-112.999829763877,-1.7598783485397));
#5834=CARTESIAN_POINT('Ctrl Pts',(-19.5,-110.044590565554,-1.84295634970223));
#5835=CARTESIAN_POINT('Ctrl Pts',(-16.5444962146153,-109.999992849754,-1.84241782580659));
#5836=CARTESIAN_POINT('Ctrl Pts',(-19.5,-112.991171615148,-1.57801081699067));
#5837=CARTESIAN_POINT('Ctrl Pts',(-19.5,-110.144230037263,-1.75197525332857));
#5838=CARTESIAN_POINT('Ctrl Pts',(-16.6516660427078,-109.999976541827,-1.76000173974572));
#5839=CARTESIAN_POINT('Ctrl Pts',(-19.5,-112.986249389692,-1.5058693702657));
#5840=CARTESIAN_POINT('Ctrl Pts',(-19.5,-110.187949454441,-1.70482429850909));
#5841=CARTESIAN_POINT('Ctrl Pts',(-16.7009884325079,-109.999969217678,-1.71745839364903));
#5842=CARTESIAN_POINT('Ctrl Pts',(-19.5,-112.975531858613,-1.36165997451602));
#5843=CARTESIAN_POINT('Ctrl Pts',(-19.5,-110.278138535025,-1.57218464266277));
#5844=CARTESIAN_POINT('Ctrl Pts',(-16.8088388634061,-109.999953678584,-1.59315234152839));
#5845=CARTESIAN_POINT('Ctrl Pts',(-19.5,-112.969742052832,-1.28956238379365));
#5846=CARTESIAN_POINT('Ctrl Pts',(-19.5,-110.324934754411,-1.48619080097002));
#5847=CARTESIAN_POINT('Ctrl Pts',(-16.868219541035,-109.999945443368,-1.51004474513582));
#5848=CARTESIAN_POINT('Ctrl Pts',(-19.5,-112.960920191473,-1.14532173153354));
#5849=CARTESIAN_POINT('Ctrl Pts',(-19.5,-110.397592333861,-1.26873559836766));
#5850=CARTESIAN_POINT('Ctrl Pts',(-16.9649792338562,-109.999932251101,-1.28757126147114));
#5851=CARTESIAN_POINT('Ctrl Pts',(-19.5,-112.95806404802,-1.07317576949094));
#5852=CARTESIAN_POINT('Ctrl Pts',(-19.4999999999996,-110.422001594761,-1.13591166547741));
#5853=CARTESIAN_POINT('Ctrl Pts',(-16.9992863852965,-109.999927765103,-1.14635219596316));
#5854=CARTESIAN_POINT('Ctrl Pts',(-19.5,-112.958016061818,-0.928790450299966));
#5855=CARTESIAN_POINT('Ctrl Pts',(-19.5000000000004,-110.422406145868,-0.867751004179269));
#5856=CARTESIAN_POINT('Ctrl Pts',(-16.9998542260842,-109.999927689389,-0.857580282052989));
#5857=CARTESIAN_POINT('Ctrl Pts',(-19.5,-112.960828724944,-0.856551018857039));
#5858=CARTESIAN_POINT('Ctrl Pts',(-19.5,-110.398355492936,-0.734425899282093));
#5859=CARTESIAN_POINT('Ctrl Pts',(-16.9660301139158,-109.999932110923,-0.715744450796804));
#5860=CARTESIAN_POINT('Ctrl Pts',(-19.5,-112.969622749834,-0.712019909284494));
#5861=CARTESIAN_POINT('Ctrl Pts',(-19.5,-110.325910420762,-0.515860298232045));
#5862=CARTESIAN_POINT('Ctrl Pts',(-16.8694815458653,-109.999945269335,-0.491978620513704));
#5863=CARTESIAN_POINT('Ctrl Pts',(-19.5,-112.97542425227,-0.63973119674263));
#5864=CARTESIAN_POINT('Ctrl Pts',(-19.5000000000001,-110.279014567801,-0.429305199942497));
#5865=CARTESIAN_POINT('Ctrl Pts',(-16.8099230380697,-109.999953525122,-0.408273754393743));
#5866=CARTESIAN_POINT('Ctrl Pts',(-19.5,-112.986176452745,-0.495167800039601));
#5867=CARTESIAN_POINT('Ctrl Pts',(-19.4999999999999,-110.188587950114,-0.295913281259317));
#5868=CARTESIAN_POINT('Ctrl Pts',(-16.7017210837189,-109.999969109764,-0.283212476689676));
#5869=CARTESIAN_POINT('Ctrl Pts',(-19.5,-112.991118555997,-0.422893257592481));
#5870=CARTESIAN_POINT('Ctrl Pts',(-19.5000000000005,-110.144750106835,-0.248555334537643));
#5871=CARTESIAN_POINT('Ctrl Pts',(-16.6522426698697,-109.999976455226,-0.240479902591688));
#5872=CARTESIAN_POINT('Ctrl Pts',(-19.5,-112.999819986014,-0.240644690936843));
#5873=CARTESIAN_POINT('Ctrl Pts',(-19.4999999999992,-110.044829996224,-0.157176714937319));
#5874=CARTESIAN_POINT('Ctrl Pts',(-16.5447381983765,-109.999992811267,-0.157710600871371));
#5875=CARTESIAN_POINT('Ctrl Pts',(-19.5,-113.001670882596,-0.130701702736794));
#5876=CARTESIAN_POINT('Ctrl Pts',(-19.499999999995,-109.994838487952,-0.129479576555088));
#5877=CARTESIAN_POINT('Ctrl Pts',(-16.4947631009191,-110.000000775553,-0.130932080694481));
#5878=CARTESIAN_POINT('Ctrl Pts',(-19.5,-112.998303161317,-0.0208462982633885));
#5879=CARTESIAN_POINT('Ctrl Pts',(-19.5000000000085,-109.953739602694,-0.11025770292768));
#5880=CARTESIAN_POINT('Ctrl Pts',(-16.4542587066167,-110.000007237571,-0.108794952059203));
#5881=CARTESIAN_POINT('Origin',(-16.5,-113.,-1.86602540378444));
#5882=CARTESIAN_POINT('Origin',(-16.5,-113.,-2.));
#5883=CARTESIAN_POINT('Origin',(-16.,-116.5,-2.));
#5884=CARTESIAN_POINT('',(0.,0.,0.));
#5885=CARTESIAN_POINT('Origin',(-16.,-116.5,-2.000025));
#5886=CARTESIAN_POINT('',(-18.,-116.5,-2.));
#5887=CARTESIAN_POINT('Origin',(-16.,-116.5,-2.));
#5888=CARTESIAN_POINT('',(-18.,-116.5,0.));
#5889=CARTESIAN_POINT('',(-18.,-116.5,-2.000025));
#5890=CARTESIAN_POINT('Origin',(-16.,-116.5,-3.05741378671474E-30));
#5891=CARTESIAN_POINT('Origin',(-28.5285484527122,-99.4077946409786,-1.99999999999999));
#5892=CARTESIAN_POINT('',(-21.7195444572929,-106.731554917665,-1.99999999999999));
#5893=CARTESIAN_POINT('',(-22.5,-91.4292857857286,-1.99999999999999));
#5894=CARTESIAN_POINT('Origin',(-28.5285484527122,-99.4077946409786,-1.99999999999999));
#5895=CARTESIAN_POINT('',(-21.7195444572929,-106.731554917665,6.01457402401214E-10));
#5896=CARTESIAN_POINT('',(-21.7195444572929,-106.731554917665,-1.99999999999999));
#5897=CARTESIAN_POINT('',(-22.5,-91.4292857857286,2.40741243048404E-32));
#5898=CARTESIAN_POINT('Origin',(-28.5285484527122,-99.4077946409786,0.));
#5899=CARTESIAN_POINT('',(-22.5,-91.4292857857286,-1.99999999999999));
#5900=CARTESIAN_POINT('Origin',(-22.5,-80.0000000000001,-1.99999999999999));
#5901=CARTESIAN_POINT('',(-22.5,-85.0000000000001,-1.99999999999999));
#5902=CARTESIAN_POINT('',(-21.25,-75.1587708172408,-2.));
#5903=CARTESIAN_POINT('Origin',(-22.5,-80.0000000000001,-1.99999999999999));
#5904=CARTESIAN_POINT('',(-22.4999999999998,-85.0000000000001,6.01457402401214E-10));
#5905=CARTESIAN_POINT('',(-22.5,-85.0000000000001,-1.99999999999999));
#5906=CARTESIAN_POINT('',(-21.2500000008195,-75.1587708175933,8.25034485174569E-13));
#5907=CARTESIAN_POINT('Origin',(-22.5,-80.0000000000001,0.));
#5908=CARTESIAN_POINT('',(-21.25,-75.1587708172408,-0.999994));
#5909=CARTESIAN_POINT('Origin',(0.,0.,-2.));
#5910=CARTESIAN_POINT('',(-12.5,-116.5,-2.));
#5911=CARTESIAN_POINT('',(-12.5,-70.,-2.));
#5912=CARTESIAN_POINT('',(-12.5,-120.,-2.));
#5913=CARTESIAN_POINT('',(-19.5,-116.5,-2.));
#5914=CARTESIAN_POINT('Origin',(-16.,-116.5,-2.));
#5915=CARTESIAN_POINT('',(-19.5,-110.,-2.));
#5916=CARTESIAN_POINT('',(-19.5,-120.,-2.));
#5917=CARTESIAN_POINT('Origin',(-12.5,-102.858571571457,-2.));
#5918=CARTESIAN_POINT('',(-22.5,-70.,-1.99999999999999));
#5919=CARTESIAN_POINT('Origin',(-12.5,-80.,-2.));
#5920=CARTESIAN_POINT('Origin',(0.,0.,0.));
#5921=CARTESIAN_POINT('',(-19.5,-116.5,-3.05741378671474E-30));
#5922=CARTESIAN_POINT('',(-12.5,-116.5,-7.22223729145213E-32));
#5923=CARTESIAN_POINT('Origin',(-16.,-116.5,-3.1537102839341E-30));
#5924=CARTESIAN_POINT('',(-12.5,-70.,-7.22223729145213E-32));
#5925=CARTESIAN_POINT('',(-12.5,-120.,-3.05741378671474E-30));
#5926=CARTESIAN_POINT('Origin',(-12.5,-80.,-7.22223729145213E-32));
#5927=CARTESIAN_POINT('',(-22.5,-70.,-3.05741378671474E-30));
#5928=CARTESIAN_POINT('',(-19.5,-110.,-7.22223729145213E-32));
#5929=CARTESIAN_POINT('Origin',(-12.5,-102.858571571457,-7.22223729145213E-32));
#5930=CARTESIAN_POINT('',(-19.5,-120.,-3.1537102839341E-30));
#5931=CARTESIAN_POINT('Origin',(-22.5,0.,2.40741243048404E-32));
#5932=CARTESIAN_POINT('Origin',(-19.5,-120.,-2.));
#5933=CARTESIAN_POINT('',(-19.5,-116.5,-2.));
#5934=CARTESIAN_POINT('',(-19.5,-110.,-2.));
#5935=CARTESIAN_POINT('Origin',(-12.5,-120.,-2.));
#5936=CARTESIAN_POINT('',(-12.5,-116.5,-2.));
#5937=CARTESIAN_POINT('',(-12.5,-70.,-2.));
#5938=CARTESIAN_POINT('Origin',(-12.5,-102.858571571457,-2.));
#5939=CARTESIAN_POINT('Origin',(-12.5,-80.,-7.22223729145213E-32));
#5940=CARTESIAN_POINT('Origin',(-16.,-116.5,-2.));
#5941=CARTESIAN_POINT('',(0.,0.,0.));
#5942=CARTESIAN_POINT('Origin',(5.,-15.2931109241333,-8.));
#5943=CARTESIAN_POINT('',(8.,-15.2931109241333,-7.));
#5944=CARTESIAN_POINT('Origin',(5.,-15.2931109241333,-7.));
#5945=CARTESIAN_POINT('',(8.,-15.2931109241333,-8.));
#5946=CARTESIAN_POINT('',(8.,-15.2931109241333,-8.));
#5947=CARTESIAN_POINT('Origin',(5.,-15.2931109241333,-8.));
#5948=CARTESIAN_POINT('Origin',(5.,-15.2931109241333,8.));
#5949=CARTESIAN_POINT('',(8.,-15.2931109241333,7.));
#5950=CARTESIAN_POINT('Origin',(5.,-15.2931109241333,7.));
#5951=CARTESIAN_POINT('',(8.,-15.2931109241333,8.));
#5952=CARTESIAN_POINT('',(8.,-15.2931109241333,8.));
#5953=CARTESIAN_POINT('Origin',(5.,-15.2931109241333,8.));
#5954=CARTESIAN_POINT('Origin',(5.,-15.2931109241333,7.));
#5955=CARTESIAN_POINT('',(7.,-15.2931109241333,-7.));
#5956=CARTESIAN_POINT('Origin',(5.,-15.2931109241333,-7.));
#5957=CARTESIAN_POINT('',(7.,-15.2931109241333,7.));
#5958=CARTESIAN_POINT('',(7.,-15.2931109241333,7.));
#5959=CARTESIAN_POINT('Origin',(5.,-15.2931109241333,7.));
#5960=CARTESIAN_POINT('Origin',(5.,-15.2931109241333,8.));
#5961=CARTESIAN_POINT('Origin',(5.,-15.2931109241333,7.));
#5962=CARTESIAN_POINT('Origin',(5.,-15.2931109241333,-8.));
#5963=CARTESIAN_POINT('Origin',(5.,-15.2931109241333,-7.));
#5964=CARTESIAN_POINT('',(0.,0.,0.));
#5965=CARTESIAN_POINT('',(10.,-8.45677694538693E-15,1.06041189457627E-15));
#5966=CARTESIAN_POINT('',(0.,0.,0.));
#5967=CARTESIAN_POINT('',(0.,0.,0.));
#5968=CARTESIAN_POINT('',(10.,-3.46944695195361E-15,-2.));
#5969=CARTESIAN_POINT('',(0.,-6.93889390390723E-15,2.));
#5970=CARTESIAN_POINT('',(10.,3.81639164714898E-14,0.));
#5971=CARTESIAN_POINT('',(-21.,-101.206889075867,5.20417042793042E-15));
#5972=CARTESIAN_POINT('',(18.6384826200919,-102.193102935886,-8.67361737988404E-16));
#5973=UNCERTAINTY_MEASURE_WITH_UNIT(LENGTH_MEASURE(0.01),#5991,
'DISTANCE_ACCURACY_VALUE',
'Maximum model space distance between geometric entities at asserted c
onnectivities');
#5974=UNCERTAINTY_MEASURE_WITH_UNIT(LENGTH_MEASURE(0.01),#5991,
'DISTANCE_ACCURACY_VALUE',
'Maximum model space distance between geometric entities at asserted c
onnectivities');
#5975=UNCERTAINTY_MEASURE_WITH_UNIT(LENGTH_MEASURE(0.01),#5991,
'DISTANCE_ACCURACY_VALUE',
'Maximum model space distance between geometric entities at asserted c
onnectivities');
#5976=UNCERTAINTY_MEASURE_WITH_UNIT(LENGTH_MEASURE(0.01),#5991,
'DISTANCE_ACCURACY_VALUE',
'Maximum model space distance between geometric entities at asserted c
onnectivities');
#5977=UNCERTAINTY_MEASURE_WITH_UNIT(LENGTH_MEASURE(0.01),#5991,
'DISTANCE_ACCURACY_VALUE',
'Maximum model space distance between geometric entities at asserted c
onnectivities');
#5978=UNCERTAINTY_MEASURE_WITH_UNIT(LENGTH_MEASURE(0.01),#5991,
'DISTANCE_ACCURACY_VALUE',
'Maximum model space distance between geometric entities at asserted c
onnectivities');
#5979=UNCERTAINTY_MEASURE_WITH_UNIT(LENGTH_MEASURE(0.01),#5991,
'DISTANCE_ACCURACY_VALUE',
'Maximum model space distance between geometric entities at asserted c
onnectivities');
#5980=UNCERTAINTY_MEASURE_WITH_UNIT(LENGTH_MEASURE(0.01),#5991,
'DISTANCE_ACCURACY_VALUE',
'Maximum model space distance between geometric entities at asserted c
onnectivities');
#5981=UNCERTAINTY_MEASURE_WITH_UNIT(LENGTH_MEASURE(0.01),#5991,
'DISTANCE_ACCURACY_VALUE',
'Maximum model space distance between geometric entities at asserted c
onnectivities');
#5982=(
GEOMETRIC_REPRESENTATION_CONTEXT(3)
GLOBAL_UNCERTAINTY_ASSIGNED_CONTEXT((#5973))
GLOBAL_UNIT_ASSIGNED_CONTEXT((#5991,#5993,#5994))
REPRESENTATION_CONTEXT('','3D')
);
#5983=(
GEOMETRIC_REPRESENTATION_CONTEXT(3)
GLOBAL_UNCERTAINTY_ASSIGNED_CONTEXT((#5974))
GLOBAL_UNIT_ASSIGNED_CONTEXT((#5991,#5993,#5994))
REPRESENTATION_CONTEXT('','3D')
);
#5984=(
GEOMETRIC_REPRESENTATION_CONTEXT(3)
GLOBAL_UNCERTAINTY_ASSIGNED_CONTEXT((#5975))
GLOBAL_UNIT_ASSIGNED_CONTEXT((#5991,#5993,#5994))
REPRESENTATION_CONTEXT('','3D')
);
#5985=(
GEOMETRIC_REPRESENTATION_CONTEXT(3)
GLOBAL_UNCERTAINTY_ASSIGNED_CONTEXT((#5976))
GLOBAL_UNIT_ASSIGNED_CONTEXT((#5991,#5993,#5994))
REPRESENTATION_CONTEXT('','3D')
);
#5986=(
GEOMETRIC_REPRESENTATION_CONTEXT(3)
GLOBAL_UNCERTAINTY_ASSIGNED_CONTEXT((#5977))
GLOBAL_UNIT_ASSIGNED_CONTEXT((#5991,#5993,#5994))
REPRESENTATION_CONTEXT('','3D')
);
#5987=(
GEOMETRIC_REPRESENTATION_CONTEXT(3)
GLOBAL_UNCERTAINTY_ASSIGNED_CONTEXT((#5978))
GLOBAL_UNIT_ASSIGNED_CONTEXT((#5991,#5993,#5994))
REPRESENTATION_CONTEXT('','3D')
);
#5988=(
GEOMETRIC_REPRESENTATION_CONTEXT(3)
GLOBAL_UNCERTAINTY_ASSIGNED_CONTEXT((#5979))
GLOBAL_UNIT_ASSIGNED_CONTEXT((#5991,#5993,#5994))
REPRESENTATION_CONTEXT('','3D')
);
#5989=(
GEOMETRIC_REPRESENTATION_CONTEXT(3)
GLOBAL_UNCERTAINTY_ASSIGNED_CONTEXT((#5980))
GLOBAL_UNIT_ASSIGNED_CONTEXT((#5991,#5993,#5994))
REPRESENTATION_CONTEXT('','3D')
);
#5990=(
GEOMETRIC_REPRESENTATION_CONTEXT(3)
GLOBAL_UNCERTAINTY_ASSIGNED_CONTEXT((#5981))
GLOBAL_UNIT_ASSIGNED_CONTEXT((#5991,#5993,#5994))
REPRESENTATION_CONTEXT('','3D')
);
#5991=(
LENGTH_UNIT()
NAMED_UNIT(*)
SI_UNIT(.MILLI.,.METRE.)
);
#5992=(
LENGTH_UNIT()
NAMED_UNIT(*)
SI_UNIT($,.METRE.)
);
#5993=(
NAMED_UNIT(*)
PLANE_ANGLE_UNIT()
SI_UNIT($,.RADIAN.)
);
#5994=(
NAMED_UNIT(*)
SI_UNIT($,.STERADIAN.)
SOLID_ANGLE_UNIT()
);
#5995=SHAPE_DEFINITION_REPRESENTATION(#6003,#6020);
#5996=SHAPE_DEFINITION_REPRESENTATION(#6004,#6021);
#5997=SHAPE_DEFINITION_REPRESENTATION(#6005,#6022);
#5998=SHAPE_DEFINITION_REPRESENTATION(#6006,#6023);
#5999=SHAPE_DEFINITION_REPRESENTATION(#6007,#6024);
#6000=SHAPE_DEFINITION_REPRESENTATION(#6008,#6025);
#6001=SHAPE_DEFINITION_REPRESENTATION(#6009,#6026);
#6002=SHAPE_DEFINITION_REPRESENTATION(#6010,#6027);
#6003=PRODUCT_DEFINITION_SHAPE('',$,#6029);
#6004=PRODUCT_DEFINITION_SHAPE('',$,#6030);
#6005=PRODUCT_DEFINITION_SHAPE('',$,#6031);
#6006=PRODUCT_DEFINITION_SHAPE('',$,#6032);
#6007=PRODUCT_DEFINITION_SHAPE('',$,#6033);
#6008=PRODUCT_DEFINITION_SHAPE('',$,#6034);
#6009=PRODUCT_DEFINITION_SHAPE('',$,#6035);
#6010=PRODUCT_DEFINITION_SHAPE('',$,#6036);
#6011=PRODUCT_DEFINITION_SHAPE($,$,#38);
#6012=PRODUCT_DEFINITION_SHAPE($,$,#39);
#6013=PRODUCT_DEFINITION_SHAPE($,$,#40);
#6014=PRODUCT_DEFINITION_SHAPE($,$,#41);
#6015=PRODUCT_DEFINITION_SHAPE($,$,#42);
#6016=PRODUCT_DEFINITION_SHAPE($,$,#43);
#6017=PRODUCT_DEFINITION_SHAPE($,$,#44);
#6018=PRODUCT_DEFINITION_SHAPE($,$,#45);
#6019=PRODUCT_DEFINITION_SHAPE($,$,#46);
#6020=SHAPE_REPRESENTATION('',(#3354,#3676,#3677,#3678,#3679,#3680,#3681,
#3682,#3683,#3684),#5982);
#6021=SHAPE_REPRESENTATION('',(#3355),#5983);
#6022=SHAPE_REPRESENTATION('',(#3437),#5984);
#6023=SHAPE_REPRESENTATION('',(#3519),#5985);
#6024=SHAPE_REPRESENTATION('',(#3540),#5986);
#6025=SHAPE_REPRESENTATION('',(#3585),#5987);
#6026=SHAPE_REPRESENTATION('',(#3638),#5988);
#6027=SHAPE_REPRESENTATION('',(#3662),#5989);
#6028=PRODUCT_DEFINITION_CONTEXT('part definition',#6054,'design');
#6029=PRODUCT_DEFINITION('Multi-Tool Pliers',
'MAS-151',#6037,#6028);
#6030=PRODUCT_DEFINITION('Pliers Jaw 1','Pliers Jaw 1',#6038,#6028);
#6031=PRODUCT_DEFINITION('Pliers Jaw 2','Pliers Jaw 2',#6039,#6028);
#6032=PRODUCT_DEFINITION('main knife','main knife',#6040,#6028);
#6033=PRODUCT_DEFINITION('serrated knife','serrated knife',#6041,#6028);
#6034=PRODUCT_DEFINITION('screw driver','screw driver',#6042,#6028);
#6035=PRODUCT_DEFINITION('bottle opener','bottle opener',#6043,#6028);
#6036=PRODUCT_DEFINITION('rivet pin','rivet pin',#6044,#6028);
#6037=PRODUCT_DEFINITION_FORMATION('',$,#6056);
#6038=PRODUCT_DEFINITION_FORMATION('',$,#6057);
#6039=PRODUCT_DEFINITION_FORMATION('',$,#6058);
#6040=PRODUCT_DEFINITION_FORMATION('',$,#6059);
#6041=PRODUCT_DEFINITION_FORMATION('',$,#6060);
#6042=PRODUCT_DEFINITION_FORMATION('',$,#6061);
#6043=PRODUCT_DEFINITION_FORMATION('',$,#6062);
#6044=PRODUCT_DEFINITION_FORMATION('',$,#6063);
#6045=PRODUCT_RELATED_PRODUCT_CATEGORY('MAS-151',
'MAS-151',(#6056));
#6046=PRODUCT_RELATED_PRODUCT_CATEGORY('Pliers Jaw 1','Pliers Jaw 1',(#6057));
#6047=PRODUCT_RELATED_PRODUCT_CATEGORY('Pliers Jaw 2','Pliers Jaw 2',(#6058));
#6048=PRODUCT_RELATED_PRODUCT_CATEGORY('main knife','main knife',(#6059));
#6049=PRODUCT_RELATED_PRODUCT_CATEGORY('serrated knife',
'serrated knife',(#6060));
#6050=PRODUCT_RELATED_PRODUCT_CATEGORY('screw driver','screw driver',(#6061));
#6051=PRODUCT_RELATED_PRODUCT_CATEGORY('bottle opener','bottle opener',
(#6062));
#6052=PRODUCT_RELATED_PRODUCT_CATEGORY('rivet pin','rivet pin',(#6063));
#6053=APPLICATION_PROTOCOL_DEFINITION('international standard',
'automotive_design',2009,#6054);
#6054=APPLICATION_CONTEXT(
'Core Data for Automotive Mechanical Design Process');
#6055=PRODUCT_CONTEXT('part definition',#6054,'mechanical');
#6056=PRODUCT('Multi-Tool Pliers','MAS-151',
'STEP AP214',(#6055));
#6057=PRODUCT('Pliers Jaw 1','Pliers Jaw 1',$,(#6055));
#6058=PRODUCT('Pliers Jaw 2','Pliers Jaw 2',$,(#6055));
#6059=PRODUCT('main knife','main knife',$,(#6055));
#6060=PRODUCT('serrated knife','serrated knife',$,(#6055));
#6061=PRODUCT('screw driver','screw driver',$,(#6055));
#6062=PRODUCT('bottle opener','bottle opener',$,(#6055));
#6063=PRODUCT('rivet pin','rivet pin',$,(#6055));
#6064=PRESENTATION_STYLE_ASSIGNMENT((#6070));
#6065=PRESENTATION_STYLE_ASSIGNMENT((#6071));
#6066=PRESENTATION_STYLE_ASSIGNMENT((#6072));
#6067=PRESENTATION_STYLE_ASSIGNMENT((#6073));
#6068=PRESENTATION_STYLE_ASSIGNMENT((#6074));
#6069=PRESENTATION_STYLE_ASSIGNMENT((#6075));
#6070=SURFACE_STYLE_USAGE(.BOTH.,#6076);
#6071=SURFACE_STYLE_USAGE(.BOTH.,#6077);
#6072=SURFACE_STYLE_USAGE(.BOTH.,#6078);
#6073=SURFACE_STYLE_USAGE(.BOTH.,#6079);
#6074=SURFACE_STYLE_USAGE(.BOTH.,#6080);
#6075=SURFACE_STYLE_USAGE(.BOTH.,#6081);
#6076=SURFACE_SIDE_STYLE('',(#6082));
#6077=SURFACE_SIDE_STYLE('',(#6083));
#6078=SURFACE_SIDE_STYLE('',(#6084));
#6079=SURFACE_SIDE_STYLE('',(#6085));
#6080=SURFACE_SIDE_STYLE('',(#6086));
#6081=SURFACE_SIDE_STYLE('',(#6087));
#6082=SURFACE_STYLE_FILL_AREA(#6088);
#6083=SURFACE_STYLE_FILL_AREA(#6089);
#6084=SURFACE_STYLE_FILL_AREA(#6090);
#6085=SURFACE_STYLE_FILL_AREA(#6091);
#6086=SURFACE_STYLE_FILL_AREA(#6092);
#6087=SURFACE_STYLE_FILL_AREA(#6093);
#6088=FILL_AREA_STYLE('Steel - Satin',(#6094));
#6089=FILL_AREA_STYLE('Opaque(61,176,222)',(#6095));
#6090=FILL_AREA_STYLE('Opaque(97,158,199)',(#6096));
#6091=FILL_AREA_STYLE('Opaque(31,36,43)',(#6097));
#6092=FILL_AREA_STYLE('Opaque(227,224,212)',(#6098));
#6093=FILL_AREA_STYLE('Opaque(122,133,145)',(#6099));
#6094=FILL_AREA_STYLE_COLOUR('Steel - Satin',#6100);
#6095=FILL_AREA_STYLE_COLOUR('Opaque(61,176,222)',#6101);
#6096=FILL_AREA_STYLE_COLOUR('Opaque(97,158,199)',#6102);
#6097=FILL_AREA_STYLE_COLOUR('Opaque(31,36,43)',#6103);
#6098=FILL_AREA_STYLE_COLOUR('Opaque(227,224,212)',#6104);
#6099=FILL_AREA_STYLE_COLOUR('Opaque(122,133,145)',#6105);
#6100=COLOUR_RGB('Steel - Satin',0.627450980392157,0.627450980392157,0.627450980392157);
#6101=COLOUR_RGB('Opaque(61,176,222)',0.23921568627451,0.690196078431373,
0.870588235294118);
#6102=COLOUR_RGB('Opaque(97,158,199)',0.380392156862745,0.619607843137255,
0.780392156862745);
#6103=COLOUR_RGB('Opaque(31,36,43)',0.12156862745098,0.141176470588235,
0.168627450980392);
#6104=COLOUR_RGB('Opaque(227,224,212)',0.890196078431372,0.87843137254902,
0.831372549019608);
#6105=COLOUR_RGB('Opaque(122,133,145)',0.47843137254902,0.52156862745098,
0.568627450980392);
ENDSEC;
END-ISO-10303-21;
